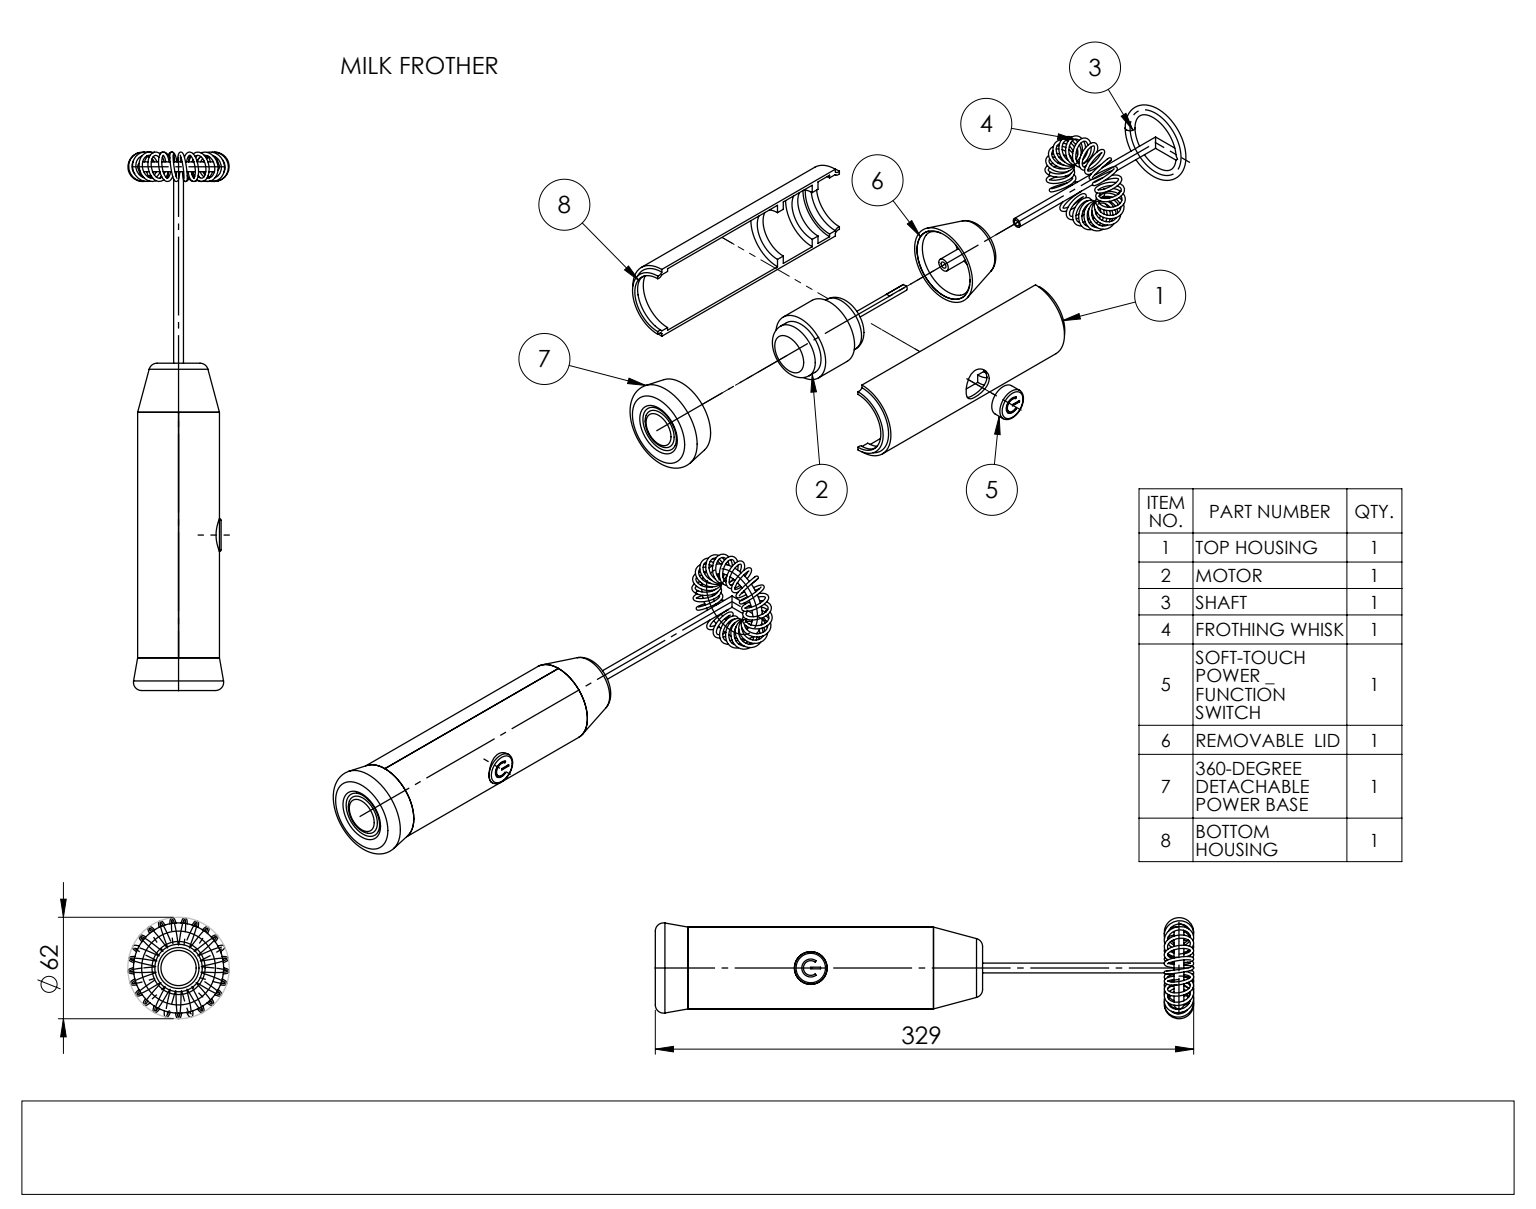
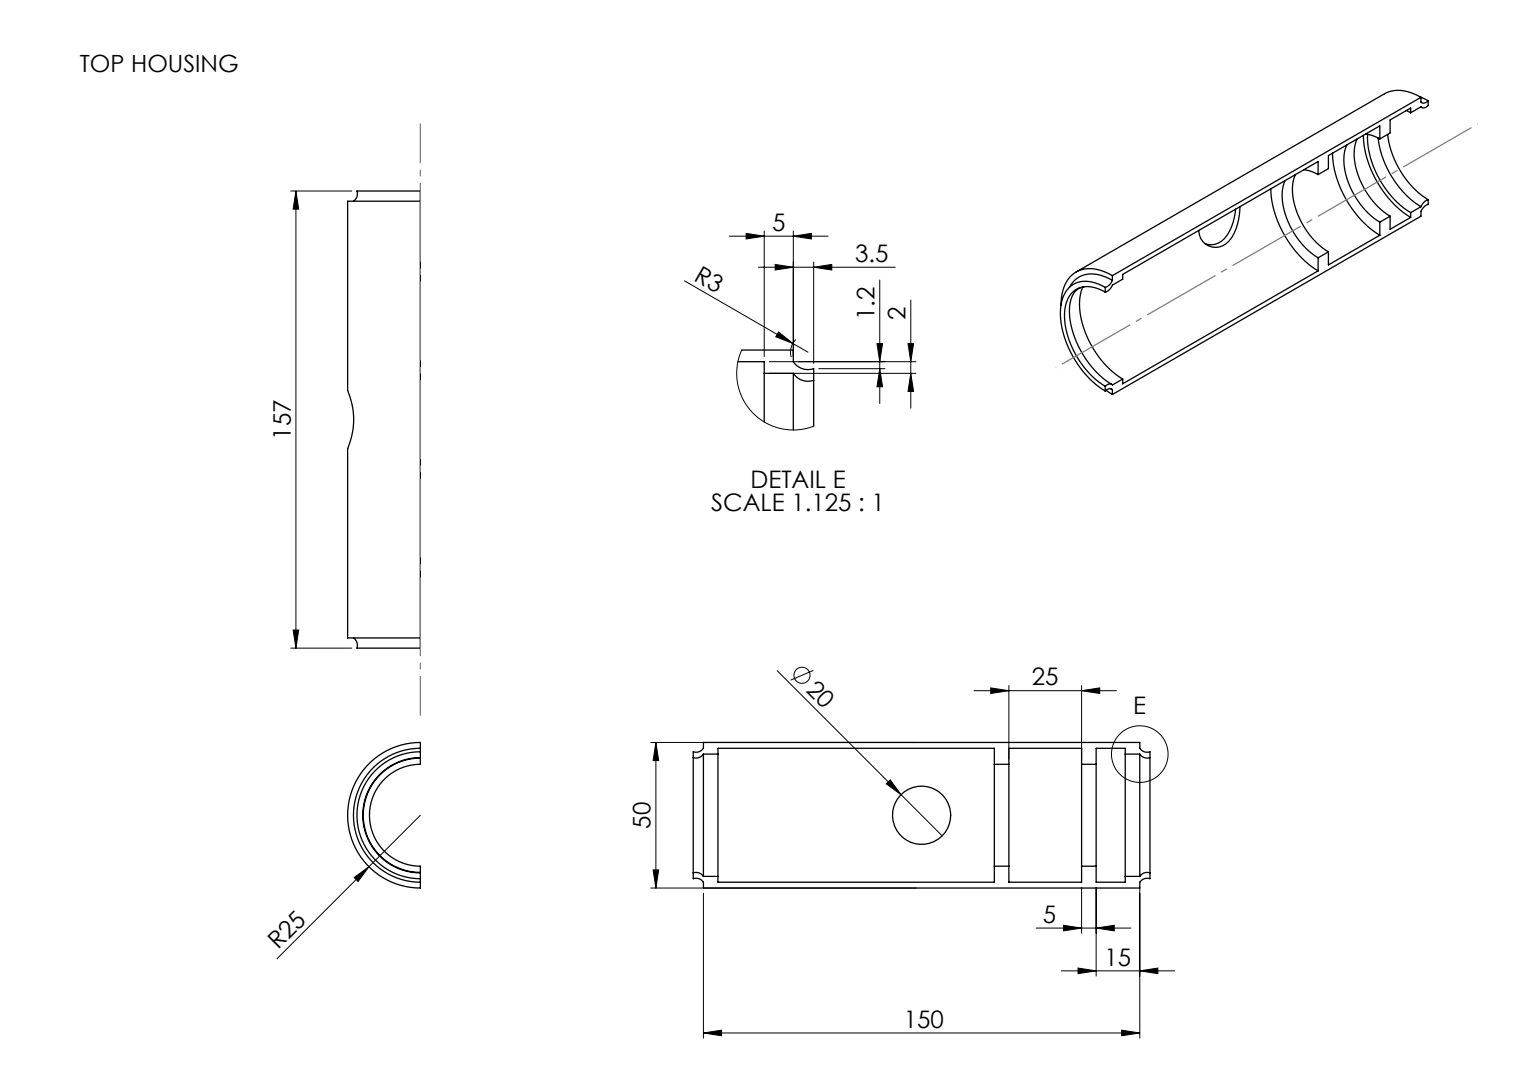
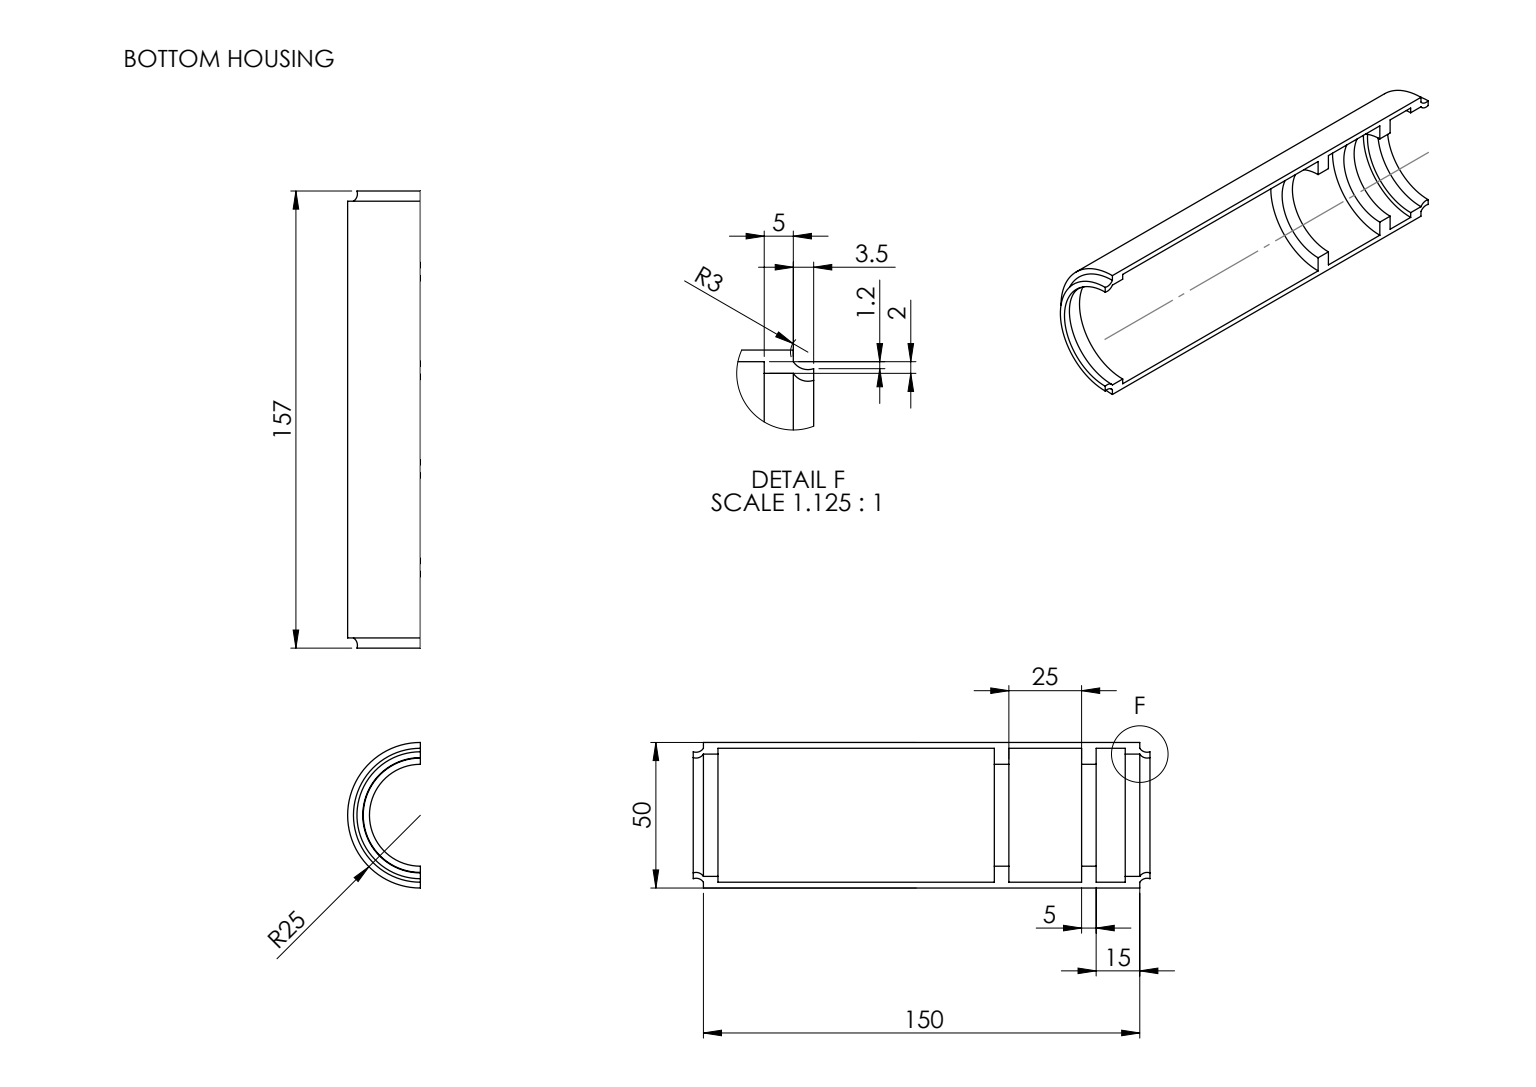
ISO-10303-21;
HEADER;
FILE_DESCRIPTION (('STEP AP214'),
    '1' );
FILE_NAME ('BR-822',
    '2026-10-08T15:02:10',
    ( '' ),
    ( '' ),
    'SwSTEP 2.0',
    'SolidWorks 2026',
    '' );
FILE_SCHEMA (( 'AUTOMOTIVE_DESIGN' ));
ENDSEC;

DATA;
#1 = CARTESIAN_POINT ( 'NONE',  ( -16.20471097821853235, -2.781505378741172319, -220.1484675126197317 ) ) ;
#2 = CARTESIAN_POINT ( 'NONE',  ( -19.86079186537285324, -0.7838168488858909821, -215.1601656726509475 ) ) ;
#3 = CARTESIAN_POINT ( 'NONE',  ( -18.57671526409105667, -15.84599122335686161, -218.9973662248357300 ) ) ;
#4 = SHAPE_REPRESENTATION_RELATIONSHIP ( 'NONE' , 'NONE' ,  #21505, #10999 ) ;
#5 = CARTESIAN_POINT ( 'NONE',  ( 13.07616324839670341, -23.69356132834180784, -230.7206382488779184 ) ) ;
#6 = CARTESIAN_POINT ( 'NONE',  ( -16.32047052250102581, 2.570795953410685009, -230.9329235942756213 ) ) ;
#7 = CARTESIAN_POINT ( 'NONE',  ( 10.40160332990717151, 27.59713857063802323, -221.5374724512453213 ) ) ;
#8 = CARTESIAN_POINT ( 'NONE',  ( -4.824452364631481416, 22.01523768541901305, -216.8350837474290245 ) ) ;
#9 = ORIENTED_EDGE ( 'NONE', *, *, #11620, .F. ) ;
#10 = CARTESIAN_POINT ( 'NONE',  ( 20.64894435305043174, -4.471500992710556233, -235.2405168901568686 ) ) ;
#11 = VERTEX_POINT ( 'NONE', #9296 ) ;
#12 = CARTESIAN_POINT ( 'NONE',  ( 12.99034161053428349, 11.71468708507361889, -230.9043293568357740 ) ) ;
#13 = CARTESIAN_POINT ( 'NONE',  ( -7.812160407601123069, 10.19183344000749081, -223.8148904943605828 ) ) ;
#14 = CARTESIAN_POINT ( 'NONE',  ( -12.30606003331388543, 10.59782772616791036, -231.0021630509705801 ) ) ;
#15 = CARTESIAN_POINT ( 'NONE',  ( -11.57846532275044460, -10.37575015818511304, -229.3776965522603462 ) ) ;
#16 = CARTESIAN_POINT ( 'NONE',  ( 2.465190328815661892E-29, 24.63401512838760610, -77.51594804401857175 ) ) ;
#17 = CARTESIAN_POINT ( 'NONE',  ( 16.21758812354607215, 4.665393561625732488, -232.5634757513959983 ) ) ;
#18 = CARTESIAN_POINT ( 'NONE',  ( -25.36936018126600345, 11.57160208538938306, -224.9662154788713622 ) ) ;
#19 = CARTESIAN_POINT ( 'NONE',  ( 16.71363093372661979, 20.70203100498337179, -215.6856694095356488 ) ) ;
#20 = CARTESIAN_POINT ( 'NONE',  ( 25.85597688020959239, 3.954559836939000039, -230.6766427064781624 ) ) ;
#21 = ADVANCED_FACE ( 'NONE', ( #14586 ), #5680, .F. ) ;
#22 = CARTESIAN_POINT ( 'NONE',  ( -4.451292041429703694, -15.86428280493796628, -231.0943874731633798 ) ) ;
#23 = ORIENTED_EDGE ( 'NONE', *, *, #2267, .F. ) ;
#24 = CARTESIAN_POINT ( 'NONE',  ( -8.978805095734141872, -14.89723076936793156, -219.0730636071341451 ) ) ;
#25 = CARTESIAN_POINT ( 'NONE',  ( -4.813101935419741295, 13.68373293383429434, -229.7840611589179503 ) ) ;
#26 = CARTESIAN_POINT ( 'NONE',  ( 1.541778504653760429, -23.48174737203985529, -233.9922866444541967 ) ) ;
#27 = CARTESIAN_POINT ( 'NONE',  ( -7.395406416482832590, 12.93623984139929739, -219.2606224730616873 ) ) ;
#28 = CARTESIAN_POINT ( 'NONE',  ( 22.70267758588118312, -6.899298642777032420, -215.6456595153534863 ) ) ;
#29 = AXIS2_PLACEMENT_3D ( 'NONE', #18064, #14475, #11199 ) ;
#30 = CARTESIAN_POINT ( 'NONE',  ( -13.52935284690462758, -5.503084506376929141, -222.3607690796775671 ) ) ;
#31 = CARTESIAN_POINT ( 'NONE',  ( -14.58575946311604277, 2.190332613129932327, -228.6717927865686590 ) ) ;
#32 = DIRECTION ( 'NONE',  ( -1.000000000000000000, 0.000000000000000000, 0.000000000000000000 ) ) ;
#33 = CARTESIAN_POINT ( 'NONE',  ( -3.139695637132168038, 25.12735071829084177, -230.1469660918596389 ) ) ;
#34 = CARTESIAN_POINT ( 'NONE',  ( 18.30177952310522471, 1.918278963380847468, -233.8574151782075887 ) ) ;
#35 = CARTESIAN_POINT ( 'NONE',  ( 7.639528166734322667, 11.92751229241157596, -224.6077814063189635 ) ) ;
#36 = CARTESIAN_POINT ( 'NONE',  ( 12.15450584778660570, 2.288537795953278220, -225.7049340319972828 ) ) ;
#37 = CARTESIAN_POINT ( 'NONE',  ( -3.630465294598614889, -13.73165509241056093, -221.1424077787270619 ) ) ;
#38 = CARTESIAN_POINT ( 'NONE',  ( 8.546572992885776543, 19.06776382077057974, -214.7173484156796519 ) ) ;
#39 = DIRECTION ( 'NONE',  ( -1.000000000000000000, 0.000000000000000000, 0.000000000000000000 ) ) ;
#40 = CARTESIAN_POINT ( 'NONE',  ( 8.654719819004025538, -19.13368099829532909, -232.5229659899653711 ) ) ;
#41 = CARTESIAN_POINT ( 'NONE',  ( -9.661739055621840322, 20.41227307912577871, -232.0920144483423257 ) ) ;
#42 = CARTESIAN_POINT ( 'NONE',  ( 3.192353461299334061, 22.13718518159985393, -217.1103300728619843 ) ) ;
#43 = CARTESIAN_POINT ( 'NONE',  ( -21.08965452150356867, -10.66825825602615296, -217.1903588586143314 ) ) ;
#44 = CARTESIAN_POINT ( 'NONE',  ( 28.65393683769942967, 4.398063292302325067, -219.1542358361629965 ) ) ;
#45 = CARTESIAN_POINT ( 'NONE',  ( 12.56362091610784049, 9.747446748398973071, -231.6428467497164547 ) ) ;
#46 = ORIENTED_EDGE ( 'NONE', *, *, #19993, .F. ) ;
#47 = CARTESIAN_POINT ( 'NONE',  ( 9.333020543840051531, 16.91085096921651143, -217.7308990335875762 ) ) ;
#48 = CARTESIAN_POINT ( 'NONE',  ( 25.31834813234691595, -9.473547856983202564, -230.2364162768838298 ) ) ;
#49 = CARTESIAN_POINT ( 'NONE',  ( 12.90474009670415967, -3.145873754258878385, -224.5449843457338375 ) ) ;
#50 = SURFACE_SIDE_STYLE ('',( #17385 ) ) ;
#51 = CARTESIAN_POINT ( 'NONE',  ( 13.61707622192329481, 14.84143455326118932, -217.6958999636067063 ) ) ;
#52 = CARTESIAN_POINT ( 'NONE',  ( -13.46535974834342220, -4.471564630954283359, -230.9063312536467834 ) ) ;
#53 = CARTESIAN_POINT ( 'NONE',  ( -6.870552667427666904, -18.85419487977974029, -216.2130481585807047 ) ) ;
#54 = CARTESIAN_POINT ( 'NONE',  ( 5.609436632608550966, -13.11664087352601094, -229.3324225951633650 ) ) ;
#55 = CARTESIAN_POINT ( 'NONE',  ( -1.364406401035816785, 24.33111505239456918, -219.5658712396381418 ) ) ;
#56 = CARTESIAN_POINT ( 'NONE',  ( 20.41968681625622040, 10.18377600976054076, -218.1989382652844256 ) ) ;
#57 = CARTESIAN_POINT ( 'NONE',  ( -26.58771759052039485, 5.114955214121561511, -218.2823714869195442 ) ) ;
#58 = CARTESIAN_POINT ( 'NONE',  ( -9.106229537879125147, 25.89784491087598184, -228.9807674929363372 ) ) ;
#59 = CARTESIAN_POINT ( 'NONE',  ( -21.75565187119130428, -2.221346625543990427, -217.0768970814220609 ) ) ;
#60 = ORIENTED_EDGE ( 'NONE', *, *, #7917, .F. ) ;
#61 = AXIS2_PLACEMENT_3D ( 'NONE', #8300, #8190, #21897 ) ;
#62 = CARTESIAN_POINT ( 'NONE',  ( -11.85645341316062051, 18.51497629668490674, -217.8828067666886454 ) ) ;
#63 = CARTESIAN_POINT ( 'NONE',  ( 15.88043104796248528, 11.88135572392608807, -216.2525917828042168 ) ) ;
#64 = CARTESIAN_POINT ( 'NONE',  ( 24.00840102751045890, 17.37402299239434100, -218.3110108534040137 ) ) ;
#65 = EDGE_CURVE ( 'NONE', #2304, #13811, #1543, .T. ) ;
#66 = CARTESIAN_POINT ( 'NONE',  ( 27.81506808824343580, -10.52944849582878106, -221.0913368219556503 ) ) ;
#67 = CARTESIAN_POINT ( 'NONE',  ( 1.322875655532295358, 1.500000000000000000, -105.0000000000000000 ) ) ;
#68 = VERTEX_POINT ( 'NONE', #19405 ) ;
#69 = CARTESIAN_POINT ( 'NONE',  ( -8.172572110426221670, 16.86653848210977813, -233.4220330256369493 ) ) ;
#70 = EDGE_CURVE ( 'NONE', #4018, #8552, #5732, .T. ) ;
#71 = CARTESIAN_POINT ( 'NONE',  ( -12.00435701841128022, -1.798699874815819166, -227.7674894005143074 ) ) ;
#72 = CARTESIAN_POINT ( 'NONE',  ( 0.000000000000000000, 24.63401512838747820, -77.51594804401857175 ) ) ;
#73 = VECTOR ( 'NONE', #4649, 1000.000000000000000 ) ;
#74 = CARTESIAN_POINT ( 'NONE',  ( 14.73698509926073186, 4.443590625350892331, -227.4062002049096236 ) ) ;
#75 = CARTESIAN_POINT ( 'NONE',  ( -13.69675006931110417, 3.702342960760605539, -228.0723273272095355 ) ) ;
#76 = CARTESIAN_POINT ( 'NONE',  ( 9.104026917753444081, -10.66572815660443041, -221.9193219976906448 ) ) ;
#77 = DIRECTION ( 'NONE',  ( 1.000000000000000000, 0.000000000000000000, 0.000000000000000000 ) ) ;
#78 = CARTESIAN_POINT ( 'NONE',  ( -27.82842955277035202, 11.70195273568964112, -227.9294339757464911 ) ) ;
#79 = PRODUCT_DEFINITION_SHAPE ( 'NONE', 'NONE',  #8374 ) ;
#80 = CARTESIAN_POINT ( 'NONE',  ( -15.15434969228324924, 4.423874646950748613, -230.6144467931089821 ) ) ;
#81 = CARTESIAN_POINT ( 'NONE',  ( 1.102456202203287550, -23.13885590315818064, -232.0370787247644557 ) ) ;
#82 = CIRCLE ( 'NONE', #20492, 19.79999999999999716 ) ;
#83 = CARTESIAN_POINT ( 'NONE',  ( 12.50000000000000355, 0.000000000000000000, -65.00000000000000000 ) ) ;
#84 = DIRECTION ( 'NONE',  ( 0.000000000000000000, 1.000000000000000000, 0.000000000000000000 ) ) ;
#85 = CARTESIAN_POINT ( 'NONE',  ( -28.13472254077564116, 12.33996625515159629, -224.9141344439281909 ) ) ;
#86 = CARTESIAN_POINT ( 'NONE',  ( 17.16551562789753049, -17.52877442517796780, -218.8649675774640286 ) ) ;
#87 = CARTESIAN_POINT ( 'NONE',  ( 12.82607305708569889, -2.701876713238477556, -226.3171933651010761 ) ) ;
#88 = AXIS2_PLACEMENT_3D ( 'NONE', #22054, #11930, #10248 ) ;
#89 = CARTESIAN_POINT ( 'NONE',  ( 18.76166303929371537, -3.000000000000002665, -225.0000000000001990 ) ) ;
#90 = CARTESIAN_POINT ( 'NONE',  ( 10.01015180241662605, 20.19019600914695900, -219.1042218506083543 ) ) ;
#91 = AXIS2_PLACEMENT_3D ( 'NONE', #18121, #12939, #8104 ) ;
#92 = CARTESIAN_POINT ( 'NONE',  ( 14.78510113471881304, 14.77128235908076803, -230.8056908117964383 ) ) ;
#93 = CARTESIAN_POINT ( 'NONE',  ( -2.652888268066178945, -28.18865072326549637, -221.4226523288203623 ) ) ;
#94 = CARTESIAN_POINT ( 'NONE',  ( 15.54083024098960486, -10.44392130763852222, -217.6620978190037476 ) ) ;
#95 = ORIENTED_EDGE ( 'NONE', *, *, #2038, .F. ) ;
#96 = CARTESIAN_POINT ( 'NONE',  ( -12.43544732248594720, 12.69828336922617318, -219.3367909706387877 ) ) ;
#97 = CARTESIAN_POINT ( 'NONE',  ( -24.92290506463145405, 6.124412323591598373, -220.3779252408000104 ) ) ;
#98 = CARTESIAN_POINT ( 'NONE',  ( -12.45629340980802269, 5.675423426979704367, -220.8874502847910719 ) ) ;
#99 = ORIENTED_EDGE ( 'NONE', *, *, #17132, .T. ) ;
#100 = CARTESIAN_POINT ( 'NONE',  ( -11.04629350503636864, -16.47921676447750983, -219.6257371594006145 ) ) ;
#101 = CARTESIAN_POINT ( 'NONE',  ( -0.6349943332661909245, -10.75744069813302417, 92.00000000000001421 ) ) ;
#102 = ORIENTED_EDGE ( 'NONE', *, *, #14912, .T. ) ;
#103 = CARTESIAN_POINT ( 'NONE',  ( 22.37138132874926910, 6.723028048925958622, -217.7073806909121743 ) ) ;
#104 = CARTESIAN_POINT ( 'NONE',  ( 19.38320831645075870, -15.01455373846949293, -219.3474289024948689 ) ) ;
#105 = CARTESIAN_POINT ( 'NONE',  ( 4.603870848087811218, 30.13529352683433515, -225.9623629403671430 ) ) ;
#106 = CARTESIAN_POINT ( 'NONE',  ( -16.65698539163286540, 11.03290537638306112, -233.6474915129378758 ) ) ;
#107 = VECTOR ( 'NONE', #10777, 1000.000000000000000 ) ;
#108 = AXIS2_PLACEMENT_3D ( 'NONE', #21877, #21538, #9854 ) ;
#109 = CARTESIAN_POINT ( 'NONE',  ( 12.66989206167516357, 2.082990619159506007, -225.6419847029432901 ) ) ;
#110 = PRODUCT_DEFINITION ( 'UNKNOWN', '', #959, #2880 ) ;
#111 = CARTESIAN_POINT ( 'NONE',  ( 7.168644370073567806, 19.32044210858112265, -233.1278450877711634 ) ) ;
#112 = CARTESIAN_POINT ( 'NONE',  ( 22.03647168420945590, 0.3315607655625663064, -232.0572713672586644 ) ) ;
#113 = CARTESIAN_POINT ( 'NONE',  ( 6.589392574981438599, -17.08498810221841069, -232.9613445306918322 ) ) ;
#114 = CARTESIAN_POINT ( 'NONE',  ( 14.31589812732703670, -5.349901619299376243, -221.2752230612865105 ) ) ;
#115 = CARTESIAN_POINT ( 'NONE',  ( 23.92685091328690916, 0.000000000000000000, 80.43141006107198621 ) ) ;
#116 = DIRECTION ( 'NONE',  ( -1.000000000000000000, 0.000000000000000000, 0.000000000000000000 ) ) ;
#117 = CARTESIAN_POINT ( 'NONE',  ( 15.01439307471096463, 1.118969480519667048, -226.7488225241675366 ) ) ;
#118 = CARTESIAN_POINT ( 'NONE',  ( -15.02551512915570697, -20.93241195546420741, -218.9083119944682778 ) ) ;
#119 = VECTOR ( 'NONE', #1597, 1000.000000000000000 ) ;
#120 = CIRCLE ( 'NONE', #7315, 21.50000000000000711 ) ;
#121 = CARTESIAN_POINT ( 'NONE',  ( -22.13857085231108712, 6.545953331035805789, -217.2801712530867633 ) ) ;
#122 = CARTESIAN_POINT ( 'NONE',  ( -0.3197916200495275474, 16.38897215927557482, -229.9606066735827028 ) ) ;
#123 = CARTESIAN_POINT ( 'NONE',  ( 2.085064686336211892, 14.99578618537741548, -226.0985834012817861 ) ) ;
#124 = CARTESIAN_POINT ( 'NONE',  ( -27.59531865868800082, -2.367229732415436771, -222.8128998708299093 ) ) ;
#125 = CARTESIAN_POINT ( 'NONE',  ( 7.995304978256253747, 13.28024228361502779, -220.6535174700288451 ) ) ;
#126 = CARTESIAN_POINT ( 'NONE',  ( -10.95054816480499760, 8.339404316518379545, -224.1596700080921778 ) ) ;
#127 = CARTESIAN_POINT ( 'NONE',  ( -16.40443871513620522, 4.023423476741658789, -228.9829044427089002 ) ) ;
#128 = CARTESIAN_POINT ( 'NONE',  ( -11.18311023676720062, -15.30649302686804347, -231.8766562234714002 ) ) ;
#129 = CARTESIAN_POINT ( 'NONE',  ( 26.00000000000000000, -0.5000000000000000000, 0.000000000000000000 ) ) ;
#130 = CARTESIAN_POINT ( 'NONE',  ( 20.76808360334631232, 5.412616674732960931, -234.1222385626545304 ) ) ;
#131 = AXIS2_PLACEMENT_3D ( 'NONE', #8453, #22168, #4530 ) ;
#132 = CARTESIAN_POINT ( 'NONE',  ( -14.22959263369750182, 18.28478771081826793, -217.8090497856120464 ) ) ;
#133 = CIRCLE ( 'NONE', #6226, 27.49181041625929112 ) ;
#134 = CARTESIAN_POINT ( 'NONE',  ( 5.964915545484365644, 11.50358694729900577, -229.9646467236423462 ) ) ;
#135 = CARTESIAN_POINT ( 'NONE',  ( -21.08008464085897060, -0.9048411197481797119, -217.0000000010748522 ) ) ;
#136 = CARTESIAN_POINT ( 'NONE',  ( -20.47121909278842722, -2.147015668718357695, -235.2226201655121258 ) ) ;
#137 = VERTEX_POINT ( 'NONE', #405 ) ;
#138 = CARTESIAN_POINT ( 'NONE',  ( -28.43596199216294806, -10.51226423640377838, -227.0041752157952430 ) ) ;
#139 = CARTESIAN_POINT ( 'NONE',  ( -15.64710113362562183, 25.90300453978063189, -220.8637308366217269 ) ) ;
#140 = CARTESIAN_POINT ( 'NONE',  ( -5.525229149912007642, -13.32411127922494742, -220.4018445532201440 ) ) ;
#141 = CARTESIAN_POINT ( 'NONE',  ( -4.620781219515533778, 16.99182040716223696, -217.1278208835672672 ) ) ;
#142 = CARTESIAN_POINT ( 'NONE',  ( 29.03861746756086859, -6.579333063807603743, -229.8282242506458317 ) ) ;
#143 = CARTESIAN_POINT ( 'NONE',  ( -29.22168435891936156, -1.352755938724206519, -225.9547066689444250 ) ) ;
#144 = CARTESIAN_POINT ( 'NONE',  ( 29.81944548462877975, 8.043843257819576209, -228.1755181449411793 ) ) ;
#145 = FACE_OUTER_BOUND ( 'NONE', #18733, .T. ) ;
#146 = CARTESIAN_POINT ( 'NONE',  ( -0.7879796667336372851, 21.22375955577181372, -219.1554080315090118 ) ) ;
#147 = CARTESIAN_POINT ( 'NONE',  ( -29.16153046926437753, 6.356672163541281506, -226.4393515956758165 ) ) ;
#148 = CARTESIAN_POINT ( 'NONE',  ( 18.76922974182421555, 13.12635134380198210, -217.8010375391909008 ) ) ;
#149 = CARTESIAN_POINT ( 'NONE',  ( 19.55931020704464274, 3.833820734573247346, -215.4549349108404783 ) ) ;
#150 = CARTESIAN_POINT ( 'NONE',  ( 3.585135836405817233, -11.76492230538331896, -228.1718440842192024 ) ) ;
#151 = CARTESIAN_POINT ( 'NONE',  ( 1.660345614755502686, 12.19060476922103931, -223.1112690039082906 ) ) ;
#152 = AXIS2_PLACEMENT_3D ( 'NONE', #2857, #13336, #13120 ) ;
#153 = CARTESIAN_POINT ( 'NONE',  ( 1.387778780781446180E-13, -19.80000000000006111, 78.50000000000000000 ) ) ;
#154 = CARTESIAN_POINT ( 'NONE',  ( 0.5037192024386412115, -21.28831724695581684, -215.7417742237681466 ) ) ;
#155 = CARTESIAN_POINT ( 'NONE',  ( -8.317278876689359279, 23.15034512777772235, -218.2935523245793092 ) ) ;
#156 = CARTESIAN_POINT ( 'NONE',  ( 14.20064147608437821, 14.63411858269657806, -233.6150408276221242 ) ) ;
#157 = CARTESIAN_POINT ( 'NONE',  ( -26.43144772945995413, -6.745116643720071359, -219.5134289301136050 ) ) ;
#158 = CARTESIAN_POINT ( 'NONE',  ( -22.38528940623734798, 16.50235888036280230, -227.1443357386333162 ) ) ;
#159 = CARTESIAN_POINT ( 'NONE',  ( -17.89085717681497201, 10.08962028281416856, -232.3705156551908431 ) ) ;
#160 = CARTESIAN_POINT ( 'NONE',  ( 27.79670308438203108, 10.67628923451848877, -225.2981230784098727 ) ) ;
#161 = VERTEX_POINT ( 'NONE', #16052 ) ;
#162 = CARTESIAN_POINT ( 'NONE',  ( 12.23063869552301242, 12.84118223717021934, -218.8273164334868284 ) ) ;
#163 = CARTESIAN_POINT ( 'NONE',  ( 10.59565547865383728, -13.75865772189005476, -221.5384683668846435 ) ) ;
#164 = ORIENTED_EDGE ( 'NONE', *, *, #3485, .T. ) ;
#165 = CARTESIAN_POINT ( 'NONE',  ( 27.76845665997775114, -9.103683020204879739, -229.9743915588940979 ) ) ;
#166 = CARTESIAN_POINT ( 'NONE',  ( -0.6272116608575281083, 20.18031380156121202, -219.3960054794027030 ) ) ;
#167 = ORIENTED_EDGE ( 'NONE', *, *, #18433, .F. ) ;
#168 = SURFACE_STYLE_USAGE ( .BOTH. , #50 ) ;
#169 = AXIS2_PLACEMENT_3D ( 'NONE', #2504, #9798, #9382 ) ;
#170 = CARTESIAN_POINT ( 'NONE',  ( 23.04897566969193079, 17.95862962700741861, -223.6438515760422661 ) ) ;
#171 = CARTESIAN_POINT ( 'NONE',  ( -11.65988442122670676, -3.998659314375652141, -223.4258670541443621 ) ) ;
#172 = CARTESIAN_POINT ( 'NONE',  ( -5.902479482706956659, -14.78727544128710214, -218.5565286504736946 ) ) ;
#173 = CARTESIAN_POINT ( 'NONE',  ( 13.04434844185555420, -10.19049307777131297, -230.8679447648462713 ) ) ;
#174 = CARTESIAN_POINT ( 'NONE',  ( -7.366083718505351818, 19.86648438590005838, -231.8662444779758971 ) ) ;
#175 = CARTESIAN_POINT ( 'NONE',  ( 26.00000000000000000, 0.5000000000000000000, 0.000000000000000000 ) ) ;
#176 = CARTESIAN_POINT ( 'NONE',  ( 17.02590609996173754, 6.796709046606974169, -230.8496778635019098 ) ) ;
#177 = CARTESIAN_POINT ( 'NONE',  ( -13.55591840520136770, 8.363404288414606924, -231.2690188357804857 ) ) ;
#178 = CARTESIAN_POINT ( 'NONE',  ( -5.589224416770360193, 14.13652937339764115, -225.1481999119820330 ) ) ;
#179 = ORIENTED_EDGE ( 'NONE', *, *, #598, .F. ) ;
#180 = CARTESIAN_POINT ( 'NONE',  ( 5.359747511823000465, 20.14556701535824601, -232.9094821222151381 ) ) ;
#181 = CARTESIAN_POINT ( 'NONE',  ( -18.90911063232017142, 5.352531560950812839, -219.6301177803536575 ) ) ;
#182 = CARTESIAN_POINT ( 'NONE',  ( 13.85207896949186335, 7.847214149978243292, -217.3457543576531066 ) ) ;
#183 = CARTESIAN_POINT ( 'NONE',  ( 5.133806223762193532, -16.42362916962670383, -230.4968203642818310 ) ) ;
#184 = DIRECTION ( 'NONE',  ( 0.000000000000000000, 0.000000000000000000, -1.000000000000000000 ) ) ;
#185 = ORIENTED_EDGE ( 'NONE', *, *, #19709, .T. ) ;
#186 = ADVANCED_FACE ( 'NONE', ( #19627 ), #432, .T. ) ;
#187 = CARTESIAN_POINT ( 'NONE',  ( -6.101488798441174310, 11.33371047077072369, -225.3616985956418546 ) ) ;
#188 = CARTESIAN_POINT ( 'NONE',  ( -25.17982544627478703, 0.9072515815786372784, -215.5253307415545692 ) ) ;
#189 = CARTESIAN_POINT ( 'NONE',  ( 26.48152825632016061, -2.044474411990439666, -219.3412966555575565 ) ) ;
#190 = CARTESIAN_POINT ( 'NONE',  ( 25.69300549816939494, 5.947472783069708946, -230.6131061331718115 ) ) ;
#191 = FACE_OUTER_BOUND ( 'NONE', #11098, .T. ) ;
#192 = CIRCLE ( 'NONE', #12763, 23.92685091328691271 ) ;
#193 = CARTESIAN_POINT ( 'NONE',  ( 20.25084204406298127, -10.11176871144018818, -232.7817218064674591 ) ) ;
#194 = CARTESIAN_POINT ( 'NONE',  ( -8.823862513872974489, 14.92351368520778898, -217.1499513473673346 ) ) ;
#195 = CARTESIAN_POINT ( 'NONE',  ( -28.17543631911187063, 3.557555778861649642, -230.1980773687482156 ) ) ;
#196 = CARTESIAN_POINT ( 'NONE',  ( -1.432270239486107766, -17.91381153981195951, -219.1344183636291802 ) ) ;
#197 = CARTESIAN_POINT ( 'NONE',  ( 0.000000000000000000, 0.000000000000000000, 78.50000000000000000 ) ) ;
#198 = EDGE_CURVE ( 'NONE', #16686, #4564, #9428, .T. ) ;
#199 = LINE ( 'NONE', #7182, #5891 ) ;
#200 = CARTESIAN_POINT ( 'NONE',  ( -20.18153419852512442, 14.25141268122526483, -233.5059133483111964 ) ) ;
#201 = CARTESIAN_POINT ( 'NONE',  ( 23.31955656579280145, -13.39010844438576520, -228.3495985225334266 ) ) ;
#202 = CARTESIAN_POINT ( 'NONE',  ( -27.85133024402786006, -1.794102530182491773, -229.4204807338591081 ) ) ;
#203 = CARTESIAN_POINT ( 'NONE',  ( -22.92002576459826102, 9.983672621040497575, 0.6612741795047580862 ) ) ;
#204 = CARTESIAN_POINT ( 'NONE',  ( 24.14003655968566520, 13.76285650325712773, -228.1266575292093819 ) ) ;
#205 = CARTESIAN_POINT ( 'NONE',  ( -4.813101935419741295, 13.68373293383429434, -229.7840611589179503 ) ) ;
#206 = CARTESIAN_POINT ( 'NONE',  ( 17.42772712443221650, 11.35756022693713341, -231.2166398222404382 ) ) ;
#207 = CARTESIAN_POINT ( 'NONE',  ( -7.194605141218047173, -25.04260655977047278, -230.2952862975163271 ) ) ;
#208 = CIRCLE ( 'NONE', #12782, 23.00000000000000000 ) ;
#209 = CARTESIAN_POINT ( 'NONE',  ( 23.45680152528306550, 2.072154465955917235, -232.7243927205664704 ) ) ;
#210 = ORIENTED_EDGE ( 'NONE', *, *, #8940, .F. ) ;
#211 = CIRCLE ( 'NONE', #21742, 17.50000000000000711 ) ;
#212 = CARTESIAN_POINT ( 'NONE',  ( 2.579827969572558111, 15.91317371615649101, -219.7652087782269916 ) ) ;
#213 = CARTESIAN_POINT ( 'NONE',  ( -22.90687623753526125, 9.466200233939549236, -230.1557007022273638 ) ) ;
#214 = CARTESIAN_POINT ( 'NONE',  ( -30.35034897870229287, 7.696526532841741819, -221.5749790623549416 ) ) ;
#215 = VERTEX_POINT ( 'NONE', #16158 ) ;
#216 = CARTESIAN_POINT ( 'NONE',  ( -12.46707500365009480, -15.03319212650626824, -230.3369784839848933 ) ) ;
#217 = CARTESIAN_POINT ( 'NONE',  ( 0.000000000000000000, 0.000000000000000000, 75.00000000000000000 ) ) ;
#218 = ORIENTED_EDGE ( 'NONE', *, *, #19552, .T. ) ;
#219 = CARTESIAN_POINT ( 'NONE',  ( 24.78222556642275620, 17.97262539535998371, -226.6641400693514470 ) ) ;
#220 = CARTESIAN_POINT ( 'NONE',  ( 18.79065350309113214, -20.33706828427738600, -226.6662063318914591 ) ) ;
#221 = CARTESIAN_POINT ( 'NONE',  ( 23.49048926389013658, 9.645778135078892035, -218.7307869890797463 ) ) ;
#222 = CARTESIAN_POINT ( 'NONE',  ( -16.39453490553961856, 20.24836633112041184, -233.1722131570092245 ) ) ;
#223 = VECTOR ( 'NONE', #786, 1000.000000000000000 ) ;
#224 = CARTESIAN_POINT ( 'NONE',  ( 14.54999166170408209, 3.068772298969228096, -219.4784171371563275 ) ) ;
#225 = AXIS2_PLACEMENT_3D ( 'NONE', #7569, #15900, #3952 ) ;
#226 = CARTESIAN_POINT ( 'NONE',  ( 13.43170911749896490, 19.07691563292472026, -232.7497845103644636 ) ) ;
#227 = DIRECTION ( 'NONE',  ( -1.000000000000000000, 0.000000000000000000, -0.000000000000000000 ) ) ;
#228 = CARTESIAN_POINT ( 'NONE',  ( 6.427665535191954937, -16.40046818492683656, -232.5919299485929912 ) ) ;
#229 = CARTESIAN_POINT ( 'NONE',  ( 11.43609017326686050, -13.06727081285745307, -217.8903327850316316 ) ) ;
#230 = DIRECTION ( 'NONE',  ( 0.000000000000000000, -1.000000000000000000, 0.000000000000000000 ) ) ;
#231 = DIRECTION ( 'NONE',  ( -2.162300680179923768E-16, -1.000000000000000000, 0.000000000000000000 ) ) ;
#232 = CARTESIAN_POINT ( 'NONE',  ( -23.95129667199961077, 20.99391807043993552, -227.1541646794576081 ) ) ;
#233 = CARTESIAN_POINT ( 'NONE',  ( -22.78589867900506150, -1.373495078166624861, -218.8339345403132370 ) ) ;
#234 = CARTESIAN_POINT ( 'NONE',  ( 30.47710800431509170, 7.409378661937554789, -223.2007768404241688 ) ) ;
#235 = CARTESIAN_POINT ( 'NONE',  ( -1.301562195391901877, 16.19210386685474390, -220.0867867038183192 ) ) ;
#236 = CARTESIAN_POINT ( 'NONE',  ( 1.847452069095833593, 15.11597492720254543, -223.6261404253179421 ) ) ;
#237 = VERTEX_POINT ( 'NONE', #7603 ) ;
#238 = CARTESIAN_POINT ( 'NONE',  ( 14.54962894845190036, -2.357901078066860112, -232.0046840244626765 ) ) ;
#239 = CIRCLE ( 'NONE', #21420, 3.000000000000002665 ) ;
#240 = CARTESIAN_POINT ( 'NONE',  ( 22.66390650824515873, 11.48342577402021725, -231.3155567808436217 ) ) ;
#241 = CARTESIAN_POINT ( 'NONE',  ( -11.10182655035041144, 8.778638955377752850, -227.1050196202568827 ) ) ;
#242 = CARTESIAN_POINT ( 'NONE',  ( -12.26337789213896201, 9.274758280606999250, -219.9806108963443876 ) ) ;
#243 = CARTESIAN_POINT ( 'NONE',  ( -24.60063047153272819, -17.11178239752603858, -226.7032704813509554 ) ) ;
#244 = CARTESIAN_POINT ( 'NONE',  ( -16.63766460830045091, 5.158675778507696208, -232.1659425527909093 ) ) ;
#245 = CARTESIAN_POINT ( 'NONE',  ( -23.00000000000000000, 0.000000000000000000, 75.00000000000000000 ) ) ;
#246 = FACE_OUTER_BOUND ( 'NONE', #1813, .T. ) ;
#247 = CARTESIAN_POINT ( 'NONE',  ( 0.000000000000000000, 0.000000000000000000, -120.0000000000000142 ) ) ;
#248 = CARTESIAN_POINT ( 'NONE',  ( -12.04619960554013502, 10.22290173510000777, -223.1766370265664534 ) ) ;
#249 = CARTESIAN_POINT ( 'NONE',  ( 25.41781277602550304, 19.49958712797920057, -223.1230538376805441 ) ) ;
#250 = EDGE_CURVE ( 'NONE', #10146, #1916, #14804, .T. ) ;
#251 = CARTESIAN_POINT ( 'NONE',  ( 27.84414217501293010, 2.965433895642837214, -221.8999927093654492 ) ) ;
#252 = CARTESIAN_POINT ( 'NONE',  ( -13.00317340065129557, -2.278067296278880161, -219.8118061108488916 ) ) ;
#253 = EDGE_LOOP ( 'NONE', ( #21985, #19311, #21733, #15919, #6601, #3460 ) ) ;
#254 = CARTESIAN_POINT ( 'NONE',  ( -23.08212926897555306, -14.71479305961103101, -218.7697472404056214 ) ) ;
#255 = CARTESIAN_POINT ( 'NONE',  ( -7.312583518931054627, 16.22063427959223958, -217.3454962955413521 ) ) ;
#256 = CARTESIAN_POINT ( 'NONE',  ( -14.34280792637948743, -22.10828917559366147, -217.4172704053049756 ) ) ;
#257 = CARTESIAN_POINT ( 'NONE',  ( 7.743212835174657194, 11.90778931056080481, -226.0491028376908105 ) ) ;
#258 = CARTESIAN_POINT ( 'NONE',  ( 6.415926650623908323, -16.27382107952271895, -215.7995092914603674 ) ) ;
#259 = CARTESIAN_POINT ( 'NONE',  ( 14.03461600111380037, -0.1787097712218918000, -227.9951367205099473 ) ) ;
#260 = CARTESIAN_POINT ( 'NONE',  ( -28.61025869263052712, 6.891613135096296361, -222.2489362813765013 ) ) ;
#261 = CARTESIAN_POINT ( 'NONE',  ( -5.764806379010653181, 14.19340719117484007, -223.8851086052821415 ) ) ;
#262 = CARTESIAN_POINT ( 'NONE',  ( 26.06405806384012536, 5.488112530166501024, -216.5020692413490622 ) ) ;
#263 = CARTESIAN_POINT ( 'NONE',  ( -13.56011990957801139, -0.3895158544032599202, -219.3211261236655218 ) ) ;
#264 = CARTESIAN_POINT ( 'NONE',  ( 12.79953165872901266, 10.20044330008568778, -230.3912386799665626 ) ) ;
#265 = CARTESIAN_POINT ( 'NONE',  ( -0.4062606655315902371, -23.43967590431752512, -234.4451928229410100 ) ) ;
#266 = CARTESIAN_POINT ( 'NONE',  ( 5.264801124131998300, 10.54092478143144795, -226.4890466082630098 ) ) ;
#267 = CARTESIAN_POINT ( 'NONE',  ( 21.31262902390056624, 0.4111834581965390645, -232.0572713672585792 ) ) ;
#268 = CARTESIAN_POINT ( 'NONE',  ( 0.2152704783746036410, -12.84635275796930642, -226.1081088095504015 ) ) ;
#269 = CARTESIAN_POINT ( 'NONE',  ( -11.85645341316062051, 18.51497629668490674, -217.8828067666886454 ) ) ;
#270 = CARTESIAN_POINT ( 'NONE',  ( 12.74913679152205148, 9.185760885856177893, -218.6542381594888980 ) ) ;
#271 = CARTESIAN_POINT ( 'NONE',  ( -27.88251101234890328, -7.575382714962081820, -221.6715981084135478 ) ) ;
#272 = CARTESIAN_POINT ( 'NONE',  ( -18.90911063232017142, 5.352531560950812839, -219.6301177803536575 ) ) ;
#273 = EDGE_CURVE ( 'NONE', #12453, #12432, #18177, .T. ) ;
#274 = CARTESIAN_POINT ( 'NONE',  ( -4.678665819194652187, 12.50541869316310262, -220.1509054161798247 ) ) ;
#275 = CARTESIAN_POINT ( 'NONE',  ( 13.89183999136464820, 6.553741795688899252, -220.8646181278399752 ) ) ;
#276 = ORIENTED_EDGE ( 'NONE', *, *, #16709, .F. ) ;
#277 = CARTESIAN_POINT ( 'NONE',  ( 10.85678324124089755, -13.97331853324622131, -221.1336851750754420 ) ) ;
#278 = ORIENTED_EDGE ( 'NONE', *, *, #1896, .T. ) ;
#279 = CARTESIAN_POINT ( 'NONE',  ( 5.511302051500400090, -18.01881380728196902, -231.5522404100356084 ) ) ;
#280 = CARTESIAN_POINT ( 'NONE',  ( -7.928079932584687128, 26.12067226064367986, -221.2051195461628197 ) ) ;
#281 = ORIENTED_EDGE ( 'NONE', *, *, #14770, .F. ) ;
#282 = SURFACE_STYLE_FILL_AREA ( #6812 ) ;
#283 = CARTESIAN_POINT ( 'NONE',  ( 21.25094435758043332, 17.68230636442804027, -229.7964888993842010 ) ) ;
#284 = CARTESIAN_POINT ( 'NONE',  ( 26.54225689383817866, -6.924125931238839016, -230.1506921200174247 ) ) ;
#285 = CARTESIAN_POINT ( 'NONE',  ( -1.632242579688942596, -13.62074943359385415, -221.1585305289511041 ) ) ;
#286 = CARTESIAN_POINT ( 'NONE',  ( -3.300598509645395584, -18.18730530649546395, -233.4303386612170925 ) ) ;
#287 = CARTESIAN_POINT ( 'NONE',  ( -2.015708574708954259, 26.78900769828807782, -221.5371848586876808 ) ) ;
#288 = DIRECTION ( 'NONE',  ( -1.000000000000000000, 0.000000000000000000, 0.000000000000000000 ) ) ;
#289 = CARTESIAN_POINT ( 'NONE',  ( 17.24423567610276109, 8.542587572837451404, -218.6562240232607621 ) ) ;
#290 = CARTESIAN_POINT ( 'NONE',  ( -11.26857159993117996, 28.96895336474501192, -225.6039696848669678 ) ) ;
#291 = CARTESIAN_POINT ( 'NONE',  ( -8.463283775975803280, 12.69606588598396613, -228.6351674091961286 ) ) ;
#292 = ORIENTED_EDGE ( 'NONE', *, *, #18240, .F. ) ;
#293 = CARTESIAN_POINT ( 'NONE',  ( -1.433739110790628102, 17.19322394474796667, -219.1420620387681879 ) ) ;
#294 = CARTESIAN_POINT ( 'NONE',  ( -16.37512411505367282, 2.406627362596846620, -227.7341547288202719 ) ) ;
#295 = CARTESIAN_POINT ( 'NONE',  ( 7.651502705057454889, 16.60422307457919544, -215.4679461133464144 ) ) ;
#296 = CARTESIAN_POINT ( 'NONE',  ( 5.452943511046377090, -14.64908918772281865, -221.6090591728701611 ) ) ;
#297 = DIRECTION ( 'NONE',  ( 0.000000000000000000, 0.000000000000000000, 1.000000000000000000 ) ) ;
#298 = ORIENTED_EDGE ( 'NONE', *, *, #2080, .T. ) ;
#299 = CARTESIAN_POINT ( 'NONE',  ( -11.69688825528096388, 18.63404371591177622, -215.8612738028812714 ) ) ;
#300 = CARTESIAN_POINT ( 'NONE',  ( 21.83031488338151149, -1.542591969257156803, -231.3901500139511427 ) ) ;
#301 = CARTESIAN_POINT ( 'NONE',  ( 27.02029988085337919, -0.4174685747284823112, -230.1188858631967378 ) ) ;
#302 = CARTESIAN_POINT ( 'NONE',  ( 13.03557269046774714, 7.519834803053426775, -226.9490612297269081 ) ) ;
#303 = CARTESIAN_POINT ( 'NONE',  ( -13.65925618638770800, 3.289586759644148817, -222.1579143493116533 ) ) ;
#304 = CARTESIAN_POINT ( 'NONE',  ( 5.451525948382545117, -12.45300865616632713, -227.8545162512558306 ) ) ;
#305 = CARTESIAN_POINT ( 'NONE',  ( 0.000000000000000000, 0.000000000000000000, 0.000000000000000000 ) ) ;
#306 = CARTESIAN_POINT ( 'NONE',  ( -10.30050448363967419, 10.07750059423401190, -220.1837019037183723 ) ) ;
#307 = CARTESIAN_POINT ( 'NONE',  ( -12.80532875684362715, 24.61139456694233374, -232.5885756414849084 ) ) ;
#308 = CARTESIAN_POINT ( 'NONE',  ( -16.71711190488355570, 0.6105529133557690002, -230.9511258789794681 ) ) ;
#309 = CARTESIAN_POINT ( 'NONE',  ( -13.02663300398358892, -17.15584419188240162, -232.5492131852532793 ) ) ;
#310 = DIRECTION ( 'NONE',  ( -6.982962677686266711E-15, 1.000000000000000000, 0.000000000000000000 ) ) ;
#311 = DIRECTION ( 'NONE',  ( -0.1736481776669307198, 2.126576849575776229E-17, 0.9848077530122080203 ) ) ;
#312 = CARTESIAN_POINT ( 'NONE',  ( -13.65925618638770800, 3.289586759644148817, -222.1579143493116533 ) ) ;
#313 = CARTESIAN_POINT ( 'NONE',  ( 8.958604797576050771, -20.52636309154128114, -232.6441826665315205 ) ) ;
#315 = EDGE_CURVE ( 'NONE', #15629, #11616, #21983, .T. ) ;
#314 = PRESENTATION_STYLE_ASSIGNMENT (( #17535 ) ) ;
#316 = CARTESIAN_POINT ( 'NONE',  ( -24.43175472503111223, 5.307112681608126437, 8.481714195412854096 ) ) ;
#317 = CARTESIAN_POINT ( 'NONE',  ( 20.64430047260004031, 12.67811357335941480, -231.0449411089858813 ) ) ;
#318 = CARTESIAN_POINT ( 'NONE',  ( -12.38801939673351704, 9.361418580567464787, -232.8075769614211765 ) ) ;
#319 = CIRCLE ( 'NONE', #11443, 13.12488928717151637 ) ;
#320 = CARTESIAN_POINT ( 'NONE',  ( 0.000000000000000000, -23.00000000000006040, 75.00000000000000000 ) ) ;
#321 = CARTESIAN_POINT ( 'NONE',  ( 11.40028598017942230, 13.60807601628675023, -220.9105305289655519 ) ) ;
#322 = CARTESIAN_POINT ( 'NONE',  ( 2.859576749041432553, -13.55982619688326984, -227.5954719880151345 ) ) ;
#323 = CARTESIAN_POINT ( 'NONE',  ( 22.47485217157460724, -0.5904823501021798648, -216.4383471256914220 ) ) ;
#324 = VERTEX_POINT ( 'NONE', #21527 ) ;
#325 = CARTESIAN_POINT ( 'NONE',  ( -4.784012432433236484, 23.31984772163034947, -232.0554186943449508 ) ) ;
#326 = CARTESIAN_POINT ( 'NONE',  ( -27.32939371162572684, 5.861081283609568260, -224.9659309793921409 ) ) ;
#327 = CARTESIAN_POINT ( 'NONE',  ( -20.76981451797363576, 10.27702766794165257, -234.3988437453480742 ) ) ;
#328 = ORIENTED_EDGE ( 'NONE', *, *, #15715, .F. ) ;
#329 = CARTESIAN_POINT ( 'NONE',  ( -13.78780214743967214, -7.867619234746639378, -226.3818292120506044 ) ) ;
#330 = DIRECTION ( 'NONE',  ( 1.000000000000000000, 0.000000000000000000, 0.000000000000000000 ) ) ;
#331 = EDGE_LOOP ( 'NONE', ( #8318, #981, #21331, #9100 ) ) ;
#332 = CARTESIAN_POINT ( 'NONE',  ( 15.21408433160105034, 3.021350230896802103, -222.3056493717910769 ) ) ;
#333 = CARTESIAN_POINT ( 'NONE',  ( -2.392195434554431177, -23.29395655963766387, -232.4094703796048691 ) ) ;
#334 = CARTESIAN_POINT ( 'NONE',  ( 13.49011766416699842, 7.659170998773840111, -228.1905628957712793 ) ) ;
#335 = CARTESIAN_POINT ( 'NONE',  ( -19.00318367631585659, 13.14621133775862916, -233.8403879275295765 ) ) ;
#336 = AXIS2_PLACEMENT_3D ( 'NONE', #20789, #15968, #7308 ) ;
#337 = CARTESIAN_POINT ( 'NONE',  ( 22.49659352743751128, 7.060662713609715979, -215.7089950799439180 ) ) ;
#338 = CARTESIAN_POINT ( 'NONE',  ( 11.33210854356620523, 22.81476816607802149, -217.8536224460118262 ) ) ;
#339 = CARTESIAN_POINT ( 'NONE',  ( 1.322875655532295358, 1.500000000000000000, -120.0000000000000000 ) ) ;
#340 = CARTESIAN_POINT ( 'NONE',  ( 2.378655016347637652, -14.31292064579845302, -219.9942319014987220 ) ) ;
#341 = CARTESIAN_POINT ( 'NONE',  ( 14.02668320743028119, -5.282748560960272677, -221.9001732195871739 ) ) ;
#342 = CARTESIAN_POINT ( 'NONE',  ( 4.100000000000000533, 0.000000000000000000, -103.0000000000000000 ) ) ;
#343 = DIRECTION ( 'NONE',  ( -1.000000000000000000, 0.000000000000000000, 0.000000000000000000 ) ) ;
#344 = CARTESIAN_POINT ( 'NONE',  ( -22.56222084847001597, 18.89892770556097901, -231.8972396388394088 ) ) ;
#345 = CARTESIAN_POINT ( 'NONE',  ( -21.86011749369748713, -1.271659148212478385, -218.8339345395071689 ) ) ;
#346 = CARTESIAN_POINT ( 'NONE',  ( 18.30177952310522471, 1.918278963380847468, -233.8574151782075887 ) ) ;
#347 = CARTESIAN_POINT ( 'NONE',  ( -1.433739110790628102, 17.19322394474796667, -219.1420620387681879 ) ) ;
#348 = CARTESIAN_POINT ( 'NONE',  ( 5.563568780623874943, 21.86458082533069103, -218.6474243140849012 ) ) ;
#349 = ORIENTED_EDGE ( 'NONE', *, *, #13277, .F. ) ;
#350 = CARTESIAN_POINT ( 'NONE',  ( 16.60513614482655598, -17.51558294309126396, -234.8138649271977556 ) ) ;
#351 = VERTEX_POINT ( 'NONE', #11636 ) ;
#352 = B_SPLINE_CURVE_WITH_KNOTS ( 'NONE', 3,
 ( #8357, #15550, #7861, #19875, #11124, #19133, #17576, #21456, #15667, #18213, #874, #4462, #19250, #14508, #21343, #11230, #7115, #13028, #2035, #4244, #2667, #20932 ),
 .UNSPECIFIED., .F., .F.,
 ( 4, 2, 2, 2, 2, 2, 2, 2, 2, 2, 4 ),
 ( 4.821909171845164511E-17, 0.0003011134387877908666, 0.0006022268775755335946, 0.001204453755151019051, 0.001806680632726504615, 0.002408907510301990396, 0.003011134387877475744, 0.003613361265452961091, 0.004215588143028446873, 0.004516701581816189547, 0.004817815020603932220 ),
 .UNSPECIFIED. ) ;
#353 = CARTESIAN_POINT ( 'NONE',  ( 15.42212722119060864, 5.401662248084913465, -220.8333402320903645 ) ) ;
#354 = CARTESIAN_POINT ( 'NONE',  ( -14.30096418567650041, 6.974026439069829664, -228.7941652905285537 ) ) ;
#355 = CARTESIAN_POINT ( 'NONE',  ( -11.19223248830523332, 8.463078350427430507, -222.6400917074981578 ) ) ;
#356 = CARTESIAN_POINT ( 'NONE',  ( -29.74115761720981510, -1.844952462305729401, -220.6656484738778943 ) ) ;
#357 = EDGE_CURVE ( 'NONE', #14271, #20366, #5815, .T. ) ;
#358 = CARTESIAN_POINT ( 'NONE',  ( -12.90983082593748676, 14.84936372681532823, -233.8009687022269532 ) ) ;
#359 = CARTESIAN_POINT ( 'NONE',  ( 0.000000000000000000, 19.63401512838747820, 77.51594804401857175 ) ) ;
#360 = CARTESIAN_POINT ( 'NONE',  ( 29.55842656951424985, 4.785221541509360854, -220.5134865854112718 ) ) ;
#361 = CARTESIAN_POINT ( 'NONE',  ( -13.06839468023815165, 25.32320678245788059, -229.0099538679170053 ) ) ;
#362 = CARTESIAN_POINT ( 'NONE',  ( 17.65694480011521250, 15.62497337860048674, -235.2008064134603273 ) ) ;
#363 = CARTESIAN_POINT ( 'NONE',  ( -13.93333636822611155, 3.327141996558931947, -221.4468162587888287 ) ) ;
#364 = CARTESIAN_POINT ( 'NONE',  ( -21.94322237485859972, -13.31528874885349900, -215.4027562252440759 ) ) ;
#365 = B_SPLINE_CURVE_WITH_KNOTS ( 'NONE', 3,
 ( #19193, #15943, #12227, #16055, #301, #15724, #3991, #3770, #10538, #17522, #13928, #189, #519, #20763, #5345, #3654, #17407, #7171, #15832, #5457, #14265, #12340 ),
 .UNSPECIFIED., .F., .F.,
 ( 4, 2, 2, 2, 2, 2, 2, 2, 2, 2, 4 ),
 ( 0.4999446919652688059, 0.5028747035357847839, 0.5058047151063008728, 0.5087347266768169618, 0.5116647382473329397, 0.5145947498178489177, 0.5175247613883648956, 0.5204547729588808735, 0.5233847845293969625, 0.5268031313616656774, 0.5278645943380111394 ),
 .UNSPECIFIED. ) ;
#366 = CARTESIAN_POINT ( 'NONE',  ( -29.90835019730369737, -3.078401082523886334, -228.7630230812432046 ) ) ;
#367 = CARTESIAN_POINT ( 'NONE',  ( -19.40752943788874774, 15.61499612050012864, -234.7624367253776541 ) ) ;
#368 = CARTESIAN_POINT ( 'NONE',  ( -5.519971913460887336, -12.21762732219001713, -227.2962593638428359 ) ) ;
#369 = CARTESIAN_POINT ( 'NONE',  ( 8.496844655769807630, 14.66037471857024599, -219.1631158796573118 ) ) ;
#370 = CARTESIAN_POINT ( 'NONE',  ( 12.77158894069672357, -20.43488010613652150, -235.1868042311012914 ) ) ;
#371 = CARTESIAN_POINT ( 'NONE',  ( 0.000000000000000000, -17.50000000000000711, -30.00000000000000000 ) ) ;
#372 = CARTESIAN_POINT ( 'NONE',  ( -16.32047052250102581, 2.570795953410685009, -230.9329235942756213 ) ) ;
#373 = CARTESIAN_POINT ( 'NONE',  ( 1.296323513242173542, 20.09034598902932345, -230.5712631353794961 ) ) ;
#374 = CARTESIAN_POINT ( 'NONE',  ( -16.27882490622757672, 1.520697279646460398, -219.2607721384596289 ) ) ;
#375 = CARTESIAN_POINT ( 'NONE',  ( 24.57222455393806015, 12.08236629421828212, -229.7319216558644541 ) ) ;
#376 = CARTESIAN_POINT ( 'NONE',  ( -22.10934047915427314, 0.9940043559354312386, -216.9999999999999716 ) ) ;
#377 = CARTESIAN_POINT ( 'NONE',  ( -16.08690871037762449, -24.16943144049835368, -222.8355329163958345 ) ) ;
#378 = CARTESIAN_POINT ( 'NONE',  ( 2.276720224425493821, 13.44951395023989171, -229.9230017221896105 ) ) ;
#379 = FACE_OUTER_BOUND ( 'NONE', #20962, .T. ) ;
#380 = CARTESIAN_POINT ( 'NONE',  ( -1.821616882984092411, -20.20372127477041246, -234.2708619787750308 ) ) ;
#381 = CARTESIAN_POINT ( 'NONE',  ( -8.407534899841293097, 16.91942258446019665, -231.3029992963236339 ) ) ;
#382 = CARTESIAN_POINT ( 'NONE',  ( 6.566035546683759883, 15.06745272174450712, -218.8330720708048034 ) ) ;
#383 = CARTESIAN_POINT ( 'NONE',  ( -23.77327857871830830, 11.53128597905896768, -221.0855018166512025 ) ) ;
#384 = CARTESIAN_POINT ( 'NONE',  ( -13.41298582792616934, 27.85383138489214616, -228.6457525465575884 ) ) ;
#385 = CARTESIAN_POINT ( 'NONE',  ( 28.62253243811995418, 3.652502539191337494, -225.4068779441649326 ) ) ;
#386 = EDGE_LOOP ( 'NONE', ( #10513, #13863, #2222, #14894 ) ) ;
#387 = CARTESIAN_POINT ( 'NONE',  ( 6.831421020708281944, -16.86748893536391591, -229.5305077739217552 ) ) ;
#388 = CARTESIAN_POINT ( 'NONE',  ( 11.75796858304313375, -24.75965012883946414, -219.8219186532837455 ) ) ;
#389 = CARTESIAN_POINT ( 'NONE',  ( -9.175187729848801155, 26.50888816229029743, -227.9285554593684253 ) ) ;
#390 = CARTESIAN_POINT ( 'NONE',  ( 25.50000000000000000, -0.5000000000000000000, 0.000000000000000000 ) ) ;
#391 = CARTESIAN_POINT ( 'NONE',  ( 10.85888002857596923, 15.81835858589122878, -232.3913150909872627 ) ) ;
#392 = CARTESIAN_POINT ( 'NONE',  ( 19.63495056682994289, -4.096126682090319271, -232.1271738766904207 ) ) ;
#393 = CARTESIAN_POINT ( 'NONE',  ( -12.44777057840899559, -8.577008958641105352, -229.4809580173677830 ) ) ;
#394 = CARTESIAN_POINT ( 'NONE',  ( 1.729916699924999746, -18.64927252049523432, -233.5000329212076906 ) ) ;
#395 = CARTESIAN_POINT ( 'NONE',  ( -3.139695637132168038, 25.12735071829084177, -230.1469660918596389 ) ) ;
#396 = CARTESIAN_POINT ( 'NONE',  ( 19.31922195716811430, 9.600631919686000160, -218.1359845693048101 ) ) ;
#397 = CARTESIAN_POINT ( 'NONE',  ( -2.772442535524381579, 13.75675912271027457, -228.9770533867650215 ) ) ;
#398 = CARTESIAN_POINT ( 'NONE',  ( -4.285397168228398890, 18.56782363833054106, -219.4990091916804715 ) ) ;
#399 = ORIENTED_EDGE ( 'NONE', *, *, #20384, .T. ) ;
#400 = CARTESIAN_POINT ( 'NONE',  ( 8.860681144154234801, 27.11956268701432293, -229.8503778060109823 ) ) ;
#401 = CARTESIAN_POINT ( 'NONE',  ( 21.96352831578506937, -0.3315607655626218175, -233.9427286327412787 ) ) ;
#402 = CARTESIAN_POINT ( 'NONE',  ( 26.50744623559791435, 1.694095366541529923, -217.6968951254705473 ) ) ;
#403 = CARTESIAN_POINT ( 'NONE',  ( 5.920964624126254350, -19.79845160325395526, -232.2234910544682123 ) ) ;
#404 = CARTESIAN_POINT ( 'NONE',  ( 15.51129552754472307, 0.2180314803830030457, -231.3815478022924879 ) ) ;
#405 = CARTESIAN_POINT ( 'NONE',  ( 25.50000000000000000, -4.400000000000000355, -3.299999999999998490 ) ) ;
#406 = CARTESIAN_POINT ( 'NONE',  ( 4.301648988406530094, 13.23079486486395240, -223.2766268961034655 ) ) ;
#407 = CARTESIAN_POINT ( 'NONE',  ( 19.48258831087540344, -3.612136468958778934, -219.4255404790470436 ) ) ;
#408 = DIRECTION ( 'NONE',  ( 1.000000000000000000, 0.000000000000000000, 0.000000000000000000 ) ) ;
#409 = CARTESIAN_POINT ( 'NONE',  ( 15.52719855059926424, 1.633696074270991172, -221.7349885876216433 ) ) ;
#410 = CARTESIAN_POINT ( 'NONE',  ( 5.569356713096689226, -12.06902110579006226, -223.1407905962607003 ) ) ;
#411 = DIRECTION ( 'NONE',  ( 0.000000000000000000, 0.000000000000000000, 1.000000000000000000 ) ) ;
#412 = CARTESIAN_POINT ( 'NONE',  ( -13.58874046263339608, 12.73011668665171392, -216.5659449791897941 ) ) ;
#413 = CARTESIAN_POINT ( 'NONE',  ( -8.329232059016652201, 11.81357365351366617, -230.1839637212758021 ) ) ;
#414 = ORIENTED_EDGE ( 'NONE', *, *, #15901, .T. ) ;
#415 = CARTESIAN_POINT ( 'NONE',  ( -17.88126539071149779, 5.766250685202066961, -232.9050303536861293 ) ) ;
#416 = CARTESIAN_POINT ( 'NONE',  ( -10.46545893407769157, -9.768586176915025732, -226.8636372813723199 ) ) ;
#417 = CARTESIAN_POINT ( 'NONE',  ( 0.000000000000000000, 25.00000000000000000, 75.00000000000000000 ) ) ;
#418 = CARTESIAN_POINT ( 'NONE',  ( -22.24589463867734906, 5.847797018635430888, 8.118367508314726422 ) ) ;
#419 = CARTESIAN_POINT ( 'NONE',  ( -29.95012366401462955, 4.746560250930182967, -224.6954343660969471 ) ) ;
#420 = CARTESIAN_POINT ( 'NONE',  ( 5.240643865192946116, -17.54789557311951143, -217.3772572127879812 ) ) ;
#421 = DIRECTION ( 'NONE',  ( -0.2588190451025213501, 0.000000000000000000, 0.9659258262890680902 ) ) ;
#422 = CARTESIAN_POINT ( 'NONE',  ( 1.526556658859590748E-13, -21.00000000000006395, -75.00000000000000000 ) ) ;
#423 = CARTESIAN_POINT ( 'NONE',  ( 12.56556766396551872, 9.776144415819011613, -223.4791766911294815 ) ) ;
#424 = CARTESIAN_POINT ( 'NONE',  ( -14.00980274651940682, 20.05588230486321066, -234.2453272803952586 ) ) ;
#425 = CARTESIAN_POINT ( 'NONE',  ( -21.00000000000000000, 0.000000000000000000, 75.00000000000000000 ) ) ;
#426 = CARTESIAN_POINT ( 'NONE',  ( 14.72046356508972309, 21.23077830076469041, -229.4562045376679578 ) ) ;
#427 = CARTESIAN_POINT ( 'NONE',  ( 4.354371064427007276, -19.91633591276652382, -233.4790676556106348 ) ) ;
#428 = ORIENTED_EDGE ( 'NONE', *, *, #5250, .F. ) ;
#429 = CARTESIAN_POINT ( 'NONE',  ( -4.170472558179216804, 16.67407401355319152, -230.2690496885289804 ) ) ;
#430 = CARTESIAN_POINT ( 'NONE',  ( -12.04619960554013502, 10.22290173510000777, -223.1766370265664534 ) ) ;
#431 = CARTESIAN_POINT ( 'NONE',  ( -25.00745438246740804, 14.90779342625281778, -219.2410538611701156 ) ) ;
#432 = CONICAL_SURFACE ( 'NONE', #4015, 25.00000000000001066, 0.2617993877991500740 ) ;
#433 = CARTESIAN_POINT ( 'NONE',  ( -20.58582428111024853, -15.24952116403520463, -229.8418230779359135 ) ) ;
#434 = DIRECTION ( 'NONE',  ( 0.000000000000000000, -1.000000000000000000, 0.000000000000000000 ) ) ;
#435 = ORIENTED_EDGE ( 'NONE', *, *, #10221, .T. ) ;
#436 = CARTESIAN_POINT ( 'NONE',  ( 14.70646826691583975, 6.155951851203820269, -230.2899142379868920 ) ) ;
#437 = CARTESIAN_POINT ( 'NONE',  ( 6.831421020708281944, -16.86748893536391591, -229.5305077739217552 ) ) ;
#438 = CARTESIAN_POINT ( 'NONE',  ( 26.29894631880581812, 12.29609390142961090, -226.3100047295820332 ) ) ;
#439 = CARTESIAN_POINT ( 'NONE',  ( -24.24202834850560606, 19.05981756344202438, -226.6980666352953335 ) ) ;
#440 = EDGE_CURVE ( 'NONE', #17900, #18699, #12299, .T. ) ;
#441 = CARTESIAN_POINT ( 'NONE',  ( 16.77642802340811556, -0.6192566135115280535, -218.8326447441449432 ) ) ;
#442 = CIRCLE ( 'NONE', #19821, 21.63401512838748175 ) ;
#443 = CARTESIAN_POINT ( 'NONE',  ( 4.603870848087811218, 30.13529352683433515, -225.9623629403671430 ) ) ;
#444 = FACE_OUTER_BOUND ( 'NONE', #12908, .T. ) ;
#445 = CARTESIAN_POINT ( 'NONE',  ( -11.07688804854283049, -12.81333559660784971, -232.1241261852632363 ) ) ;
#446 = CARTESIAN_POINT ( 'NONE',  ( 20.25084204406298127, -10.11176871144018818, -232.7817218064674591 ) ) ;
#447 = CARTESIAN_POINT ( 'NONE',  ( 1.526556658859590243E-13, -22.63401512838748175, -77.51594804401857175 ) ) ;
#448 = LINE ( 'NONE', #14302, #21639 ) ;
#449 = CARTESIAN_POINT ( 'NONE',  ( -18.67456582549428390, 11.07053394491094345, -214.7114755712704550 ) ) ;
#450 = CARTESIAN_POINT ( 'NONE',  ( -16.09675311661892039, -3.241155435977624677, -226.6155721728984531 ) ) ;
#451 = CARTESIAN_POINT ( 'NONE',  ( -17.39737143130126285, 7.531548707695031375, -232.0788227848755696 ) ) ;
#452 = CARTESIAN_POINT ( 'NONE',  ( 3.219568897812384645, 28.82511222849302257, -221.5626884747494216 ) ) ;
#453 = CARTESIAN_POINT ( 'NONE',  ( -2.125813515909480866, 15.68152656492264363, -220.3943115937447317 ) ) ;
#454 = ORIENTED_EDGE ( 'NONE', *, *, #861, .T. ) ;
#455 = CARTESIAN_POINT ( 'NONE',  ( 20.57969228301723419, -8.207465571703625784, -214.6085555290863454 ) ) ;
#456 = ORIENTED_EDGE ( 'NONE', *, *, #16713, .T. ) ;
#457 = CARTESIAN_POINT ( 'NONE',  ( 28.02123297569005089, 5.903198806000402143, -227.5759114383273811 ) ) ;
#458 = CIRCLE ( 'NONE', #800, 23.00000000000000000 ) ;
#459 = CARTESIAN_POINT ( 'NONE',  ( -12.39195900010699702, 23.13258866008456138, -233.4668451572263166 ) ) ;
#460 = CARTESIAN_POINT ( 'NONE',  ( -15.10760069511485604, 3.026516874529453283, -224.5685390982118861 ) ) ;
#461 = CARTESIAN_POINT ( 'NONE',  ( -15.34124043857492303, -4.213426711746545372, -218.8308339851419078 ) ) ;
#462 = CARTESIAN_POINT ( 'NONE',  ( -19.25929423112888017, 9.818144317380269825, -216.1837936240308409 ) ) ;
#463 = CARTESIAN_POINT ( 'NONE',  ( 1.526556658859590243E-13, -22.63401512838748175, 77.51594804401857175 ) ) ;
#464 = EDGE_CURVE ( 'NONE', #19761, #19544, #19810, .T. ) ;
#465 = CARTESIAN_POINT ( 'NONE',  ( 23.21336156720804667, 12.57464006230432574, -232.9346648124233070 ) ) ;
#466 = CARTESIAN_POINT ( 'NONE',  ( -13.01542355754912172, 26.77630951171455820, -225.1545229496516356 ) ) ;
#467 = CARTESIAN_POINT ( 'NONE',  ( 11.17228388010293649, 5.622653638471959425, -222.3672781564363845 ) ) ;
#468 = CARTESIAN_POINT ( 'NONE',  ( -21.89065952084848021, -0.9940043559354364566, -216.9999999999999716 ) ) ;
#469 = CONICAL_SURFACE ( 'NONE', #7660, 23.06814834742187514, 0.2617993877991500740 ) ;
#470 = CARTESIAN_POINT ( 'NONE',  ( -19.24125987773642166, -8.201885216777814236, -235.2928755229699789 ) ) ;
#471 = AXIS2_PLACEMENT_3D ( 'NONE', #20639, #5224, #4585 ) ;
#472 = CARTESIAN_POINT ( 'NONE',  ( -19.29805292978571885, -8.785194383212417080, -233.3520286081516133 ) ) ;
#473 = EDGE_CURVE ( 'NONE', #16430, #17437, #6541, .T. ) ;
#474 = CARTESIAN_POINT ( 'NONE',  ( -1.973648319964989462, 15.33498294326524203, -220.9958390492969329 ) ) ;
#475 = CARTESIAN_POINT ( 'NONE',  ( -7.460068573003235670, -29.58770008691625364, -228.1902472473001637 ) ) ;
#476 = CARTESIAN_POINT ( 'NONE',  ( 4.484811161826725900, 15.38298568785217313, -219.4617573400562662 ) ) ;
#477 = CARTESIAN_POINT ( 'NONE',  ( 3.668385877085885927, -11.51845067838601366, -222.7629028536941291 ) ) ;
#478 = CARTESIAN_POINT ( 'NONE',  ( 0.000000000000000000, 0.000000000000000000, 69.99999999999998579 ) ) ;
#479 = CARTESIAN_POINT ( 'NONE',  ( 29.47107563651793427, 6.731311671946880182, -220.0565342412898815 ) ) ;
#480 = CARTESIAN_POINT ( 'NONE',  ( 30.39189047201120175, -1.943849802383817993, -228.0804048816970919 ) ) ;
#481 = CARTESIAN_POINT ( 'NONE',  ( -4.285397168228398890, 18.56782363833054106, -219.4990091916804715 ) ) ;
#482 = CARTESIAN_POINT ( 'NONE',  ( 17.34461553379066601, 6.893916422670210764, -233.3442385185644525 ) ) ;
#483 = CARTESIAN_POINT ( 'NONE',  ( 24.42567939027770407, 10.22651298688739097, -219.4562066833365748 ) ) ;
#484 = CARTESIAN_POINT ( 'NONE',  ( -13.44952714103469305, -17.53057434768947331, -217.9956016333683237 ) ) ;
#485 = EDGE_CURVE ( 'NONE', #10116, #8679, #18757, .T. ) ;
#486 = CARTESIAN_POINT ( 'NONE',  ( 1.220475224794998370, 29.83033731899746144, -230.4224274340063801 ) ) ;
#487 = AXIS2_PLACEMENT_3D ( 'NONE', #4624, #8133, #8020 ) ;
#488 = CIRCLE ( 'NONE', #9121, 3.000000000000002665 ) ;
#489 = CARTESIAN_POINT ( 'NONE',  ( 0.000000000000000000, 0.000000000000000000, 75.01817430661621700 ) ) ;
#490 = CARTESIAN_POINT ( 'NONE',  ( -3.608027314846280031, -12.96557536209330763, -219.9492366723279702 ) ) ;
#491 = CARTESIAN_POINT ( 'NONE',  ( -7.240690404266621805, 13.01623002570985044, -225.3000933658701967 ) ) ;
#492 = CARTESIAN_POINT ( 'NONE',  ( 23.22505041959077232, 19.39625294115234055, -221.5972645870541555 ) ) ;
#493 = CARTESIAN_POINT ( 'NONE',  ( -11.82020046940938407, 10.16362659047642758, -224.3364193436540575 ) ) ;
#494 = CARTESIAN_POINT ( 'NONE',  ( -3.309130212696198559, 28.80211350556483296, -217.4284252357080334 ) ) ;
#495 = CARTESIAN_POINT ( 'NONE',  ( 14.70646826691583975, 6.155951851203820269, -230.2899142379868920 ) ) ;
#496 = CARTESIAN_POINT ( 'NONE',  ( 11.33829581046623858, -17.80819325066959635, -230.7883484307220385 ) ) ;
#497 = VERTEX_POINT ( 'NONE', #16816 ) ;
#498 = CARTESIAN_POINT ( 'NONE',  ( 11.72194121175188997, -15.95900783718691507, -217.6519982781775013 ) ) ;
#499 = CARTESIAN_POINT ( 'NONE',  ( -6.901278853520646628, 15.41233971300566807, -220.5972764307651346 ) ) ;
#500 = CARTESIAN_POINT ( 'NONE',  ( -17.50000000000001066, 2.143131898507869431E-15, -30.00000000000000000 ) ) ;
#501 = CARTESIAN_POINT ( 'NONE',  ( 17.60676319847677007, 21.31475060840986302, -219.8266339603936785 ) ) ;
#502 = CARTESIAN_POINT ( 'NONE',  ( 24.56541673123750158, -5.996287403333383281, -231.6940117905984664 ) ) ;
#503 = CARTESIAN_POINT ( 'NONE',  ( -15.22366728182010043, -5.552021002219007961, -230.2511309519622671 ) ) ;
#504 = CARTESIAN_POINT ( 'NONE',  ( -7.800954605602409053, -29.95157606033723496, -226.5906573908930000 ) ) ;
#505 = CARTESIAN_POINT ( 'NONE',  ( -5.125319492185865577, 20.53749879880200524, -218.7557759432853288 ) ) ;
#506 = CARTESIAN_POINT ( 'NONE',  ( 22.56777165119825668, 0.000000000000000000, 90.00000000000000000 ) ) ;
#507 = CARTESIAN_POINT ( 'NONE',  ( 20.22510869507564024, 17.05975164568011238, -220.7829296213589316 ) ) ;
#508 = CARTESIAN_POINT ( 'NONE',  ( -17.75316132689678383, 25.03468689048078843, -222.1645193425721061 ) ) ;
#509 = CARTESIAN_POINT ( 'NONE',  ( -9.115411286166651195, 13.66191091052436235, -230.3338332872444312 ) ) ;
#510 = ORIENTED_EDGE ( 'NONE', *, *, #7205, .T. ) ;
#511 = CARTESIAN_POINT ( 'NONE',  ( 6.040050017043670394, 13.67534390435379699, -220.4759402345340504 ) ) ;
#512 = CARTESIAN_POINT ( 'NONE',  ( -23.67953786836281083, 9.946055673977088674, -229.5560005648173671 ) ) ;
#513 = CARTESIAN_POINT ( 'NONE',  ( 20.64287812348744566, 0.2024751443801864337, -216.7518974727033481 ) ) ;
#514 = CARTESIAN_POINT ( 'NONE',  ( 15.69671663880151868, -19.77919342852767315, -217.9503656454650411 ) ) ;
#515 = LINE ( 'NONE', #19075, #11094 ) ;
#516 = ORIENTED_EDGE ( 'NONE', *, *, #704, .F. ) ;
#517 = CARTESIAN_POINT ( 'NONE',  ( 5.331555957413248059, 27.50712867803999728, -219.0801070358024276 ) ) ;
#518 = CARTESIAN_POINT ( 'NONE',  ( 24.34559900986324621, -8.951716371391148286, -220.6604487471163623 ) ) ;
#519 = CARTESIAN_POINT ( 'NONE',  ( 25.54997870115619207, -2.097555195297153841, -218.7002440566220400 ) ) ;
#520 = CARTESIAN_POINT ( 'NONE',  ( 4.201723131641114328, -20.76291977712905279, -215.9522215885928347 ) ) ;
#521 = CARTESIAN_POINT ( 'NONE',  ( -22.17339560624464312, 16.26550580028390769, -232.0582861498566274 ) ) ;
#522 = AXIS2_PLACEMENT_3D ( 'NONE', #21767, #13572, #13228 ) ;
#523 = CARTESIAN_POINT ( 'NONE',  ( -11.40916210110096962, 20.01996232974788725, -234.3205435716851923 ) ) ;
#524 = CARTESIAN_POINT ( 'NONE',  ( -9.443239614166923701, 9.388015667058336788, -222.3195230688234290 ) ) ;
#525 = CARTESIAN_POINT ( 'NONE',  ( -24.95227886253013239, -16.82584358170602101, -223.8363818545792299 ) ) ;
#526 = LINE ( 'NONE', #7615, #8756 ) ;
#527 = CARTESIAN_POINT ( 'NONE',  ( 0.000000000000000000, 0.000000000000000000, 93.00000000000000000 ) ) ;
#528 = CARTESIAN_POINT ( 'NONE',  ( -15.48255455842386219, 10.01793346089237069, -233.1197357361336913 ) ) ;
#529 = CARTESIAN_POINT ( 'NONE',  ( -0.3008257096753846893, -14.77709807386645480, -230.6673697011181048 ) ) ;
#530 = SURFACE_SIDE_STYLE ('',( #12575 ) ) ;
#531 = CARTESIAN_POINT ( 'NONE',  ( 17.24423567610276109, 8.542587572837451404, -218.6562240232607621 ) ) ;
#532 = CARTESIAN_POINT ( 'NONE',  ( -8.894613172508529786, 25.42460746921206294, -232.3150764041658363 ) ) ;
#533 = CARTESIAN_POINT ( 'NONE',  ( 13.70753084697862612, 0.1061737631881888994, -227.9987150399367408 ) ) ;
#534 = CARTESIAN_POINT ( 'NONE',  ( 10.64724148863252395, 12.28344647332184181, -223.6549461381946173 ) ) ;
#535 = CARTESIAN_POINT ( 'NONE',  ( 2.980115756258533644, -14.12936798750240008, -229.0659090661425807 ) ) ;
#536 = EDGE_LOOP ( 'NONE', ( #20404, #210, #5432, #5454, #20475, #13502 ) ) ;
#537 = CARTESIAN_POINT ( 'NONE',  ( -8.857704405076667342, 24.20848540845601704, -218.8859504303524091 ) ) ;
#538 = CARTESIAN_POINT ( 'NONE',  ( -13.06839468023815165, 25.32320678245788059, -229.0099538679170053 ) ) ;
#539 = CARTESIAN_POINT ( 'NONE',  ( -27.12694304224540076, 7.756125161462346540, -217.3817363082233101 ) ) ;
#540 = AXIS2_PLACEMENT_3D ( 'NONE', #11823, #9916, #17115 ) ;
#541 = CARTESIAN_POINT ( 'NONE',  ( -14.65844530258765310, -17.20867344037294444, -230.8340913472024170 ) ) ;
#542 = CARTESIAN_POINT ( 'NONE',  ( 1.665334536937735820E-13, -23.00000000000006040, 69.99999999999998579 ) ) ;
#543 = ORIENTED_EDGE ( 'NONE', *, *, #7416, .T. ) ;
#544 = PRESENTATION_LAYER_ASSIGNMENT (  '', '', ( #18518 ) ) ;
#545 = CARTESIAN_POINT ( 'NONE',  ( -25.29098058636142810, 5.014641116111857144, -217.4658967307323110 ) ) ;
#546 = CARTESIAN_POINT ( 'NONE',  ( 8.290903921942224031, -23.90349455650518351, -230.1727405421096364 ) ) ;
#547 = CARTESIAN_POINT ( 'NONE',  ( 10.78187269046063435, 10.73871010366167944, -221.9206544238666368 ) ) ;
#548 = CARTESIAN_POINT ( 'NONE',  ( -8.501641725227710111, 25.47064987787527102, -217.3358698761548737 ) ) ;
#549 = CARTESIAN_POINT ( 'NONE',  ( -15.60078324628501356, 3.527872497691606934, -227.4630248446626695 ) ) ;
#550 = EDGE_CURVE ( 'NONE', #16938, #19932, #17685, .T. ) ;
#551 = CARTESIAN_POINT ( 'NONE',  ( 4.484811161826725900, 15.38298568785217313, -219.4617573400562662 ) ) ;
#552 = CARTESIAN_POINT ( 'NONE',  ( -10.76794919243112325, -2.704190363445815236E-15, 92.00000000000000000 ) ) ;
#553 = AXIS2_PLACEMENT_3D ( 'NONE', #16638, #4473, #5947 ) ;
#554 = CARTESIAN_POINT ( 'NONE',  ( -15.62091161899253855, -26.00636881980398840, -222.1463585103649905 ) ) ;
#555 = PRESENTATION_LAYER_ASSIGNMENT (  '', '', ( #17096 ) ) ;
#556 = CARTESIAN_POINT ( 'NONE',  ( 17.28140336138120858, -11.48510652344925020, -216.9852223368602893 ) ) ;
#557 = DIRECTION ( 'NONE',  ( 0.000000000000000000, 0.000000000000000000, -1.000000000000000000 ) ) ;
#558 = DIRECTION ( 'NONE',  ( -0.000000000000000000, -1.000000000000000000, -0.000000000000000000 ) ) ;
#559 = CARTESIAN_POINT ( 'NONE',  ( -14.08083899843152231, 10.81596681319144970, -234.3239311387574446 ) ) ;
#560 = CARTESIAN_POINT ( 'NONE',  ( -27.33303184979533285, -3.055344081261842870, -227.4850045670461043 ) ) ;
#561 = CARTESIAN_POINT ( 'NONE',  ( -13.31590776630363315, 5.340120742929252096, -225.6956515496373186 ) ) ;
#562 = CARTESIAN_POINT ( 'NONE',  ( 8.379126514044342500, 15.76264856365358646, -232.1787896114811360 ) ) ;
#563 = CARTESIAN_POINT ( 'NONE',  ( -1.238249567024760189, 29.30580384236933966, -223.2399636023643836 ) ) ;
#564 = ORIENTED_EDGE ( 'NONE', *, *, #4047, .T. ) ;
#565 = CARTESIAN_POINT ( 'NONE',  ( 19.43707201973751708, -21.22621598813149646, -232.3303264720597667 ) ) ;
#566 = VERTEX_POINT ( 'NONE', #2846 ) ;
#567 = CARTESIAN_POINT ( 'NONE',  ( 18.46552355142154411, 5.019711608606525211, -231.5099115070375433 ) ) ;
#568 = CARTESIAN_POINT ( 'NONE',  ( -4.531689447889125866, 14.11317536318881416, -231.6806015375303502 ) ) ;
#569 = CARTESIAN_POINT ( 'NONE',  ( -6.111257124579617894, 15.89946952501658295, -216.3497764690875727 ) ) ;
#570 = CARTESIAN_POINT ( 'NONE',  ( -14.31049420963804586, -8.435107166214018903, -218.7432863707801403 ) ) ;
#571 = CARTESIAN_POINT ( 'NONE',  ( -9.171998067665157350, 9.395241133357435714, -226.3428046914542051 ) ) ;
#572 = LINE ( 'NONE', #18015, #14095 ) ;
#573 = PRESENTATION_LAYER_ASSIGNMENT (  '', '', ( #14611 ) ) ;
#574 = DIRECTION ( 'NONE',  ( -1.000000000000000000, 0.000000000000000000, 0.000000000000000000 ) ) ;
#575 = CARTESIAN_POINT ( 'NONE',  ( -12.96364545172611571, 10.77137376900670063, -221.1208843751685720 ) ) ;
#576 = CARTESIAN_POINT ( 'NONE',  ( -19.50431861204945605, -0.7624880359591150736, -219.4666829195064395 ) ) ;
#577 = CARTESIAN_POINT ( 'NONE',  ( -14.87984907657228639, 0.2138881189739126887, -228.7773920408832282 ) ) ;
#578 = CARTESIAN_POINT ( 'NONE',  ( 7.995304978256253747, 13.28024228361502779, -220.6535174700288451 ) ) ;
#579 = CARTESIAN_POINT ( 'NONE',  ( -24.09642229725868745, -17.04339013636034750, -228.1169379854252384 ) ) ;
#580 = VERTEX_POINT ( 'NONE', #8267 ) ;
#581 = CARTESIAN_POINT ( 'NONE',  ( -6.072587425033909803, 24.65158735603439055, -217.4249768037189767 ) ) ;
#582 = CARTESIAN_POINT ( 'NONE',  ( -5.636842872076440081, -13.76003991320737541, -219.7405193562604495 ) ) ;
#583 = CARTESIAN_POINT ( 'NONE',  ( 16.54345861550681107, 19.37554510112122230, -218.2240151908141002 ) ) ;
#584 = CARTESIAN_POINT ( 'NONE',  ( 6.919598145955467849, -31.16410449029495311, -226.5345828574877487 ) ) ;
#585 = CARTESIAN_POINT ( 'NONE',  ( 0.000000000000000000, 0.000000000000000000, 75.00000000000000000 ) ) ;
#586 = EDGE_CURVE ( 'NONE', #10093, #20645, #8701, .T. ) ;
#587 = CARTESIAN_POINT ( 'NONE',  ( -9.954421844142357756, 11.21484508112568079, -226.0177122452137439 ) ) ;
#588 = DIRECTION ( 'NONE',  ( 0.000000000000000000, 0.000000000000000000, -1.000000000000000000 ) ) ;
#589 = CARTESIAN_POINT ( 'NONE',  ( 21.96352831578812115, -0.3315607655626495731, -233.9427286327413356 ) ) ;
#590 = CARTESIAN_POINT ( 'NONE',  ( 13.50603691942335693, 22.79443449215731832, -229.7689193854997995 ) ) ;
#591 = CARTESIAN_POINT ( 'NONE',  ( -12.33203608746942237, 8.428128317385924717, -222.9277009507565026 ) ) ;
#592 = CARTESIAN_POINT ( 'NONE',  ( 21.31262902390056624, 0.4111834581965390645, -232.0572713672585792 ) ) ;
#593 = CARTESIAN_POINT ( 'NONE',  ( -9.981957700435337699, -28.23530775694580441, -222.3321348641582347 ) ) ;
#594 = CARTESIAN_POINT ( 'NONE',  ( 13.70863938672594529, 6.616599615120571265, -232.1343637516268643 ) ) ;
#595 = DIRECTION ( 'NONE',  ( 0.000000000000000000, 0.000000000000000000, 1.000000000000000000 ) ) ;
#596 = CARTESIAN_POINT ( 'NONE',  ( 0.4504461526642338232, -19.62726417856956473, -215.9916429883993487 ) ) ;
#597 = CARTESIAN_POINT ( 'NONE',  ( 2.893760225568064115, 14.39521026618305477, -227.6654023557511550 ) ) ;
#598 = EDGE_CURVE ( 'NONE', #15940, #3862, #788, .T. ) ;
#599 = CARTESIAN_POINT ( 'NONE',  ( 14.69853173970351179, 23.44775873627089524, -231.2711109634281001 ) ) ;
#600 = CARTESIAN_POINT ( 'NONE',  ( -8.892156391762910062, 11.89593067802204551, -225.4519868197583889 ) ) ;
#601 = CARTESIAN_POINT ( 'NONE',  ( -4.154119475380428916, 11.54776298361823095, -227.0876712548254943 ) ) ;
#602 = CARTESIAN_POINT ( 'NONE',  ( 15.28706223449149348, 2.473424253736659306, -227.9634568993954531 ) ) ;
#603 = CARTESIAN_POINT ( 'NONE',  ( 9.097575839043912538, -18.13002900832716335, -219.2719510042808224 ) ) ;
#604 = ORIENTED_EDGE ( 'NONE', *, *, #18360, .F. ) ;
#605 = CARTESIAN_POINT ( 'NONE',  ( 13.17817051516727922, -26.22376201054615308, -223.3126545406654486 ) ) ;
#606 = CARTESIAN_POINT ( 'NONE',  ( -6.769588938507062004, 18.22485903270490937, -231.3660928915624879 ) ) ;
#607 = DIRECTION ( 'NONE',  ( -0.000000000000000000, -0.000000000000000000, 1.000000000000000000 ) ) ;
#608 = CARTESIAN_POINT ( 'NONE',  ( 27.04607490430786854, 4.607450003618843049, -220.3758934308003461 ) ) ;
#609 = CARTESIAN_POINT ( 'NONE',  ( 28.52058947142581502, -1.755848367977142610, -221.9695116608532715 ) ) ;
#610 = CARTESIAN_POINT ( 'NONE',  ( -20.11874861854083463, -21.11755179634840474, -229.7504124090357323 ) ) ;
#611 = CARTESIAN_POINT ( 'NONE',  ( 1.623338700557370951, -21.82196275546919040, -234.1129525514646730 ) ) ;
#612 = CARTESIAN_POINT ( 'NONE',  ( 8.829458998963966465, 22.90677303676718779, -219.2026791561175685 ) ) ;
#613 = CARTESIAN_POINT ( 'NONE',  ( -19.79999999999999716, 0.000000000000000000, -78.50000000000000000 ) ) ;
#614 = CARTESIAN_POINT ( 'NONE',  ( -28.99982533490676317, 5.894721259135065949, -231.5937499788843468 ) ) ;
#615 = CARTESIAN_POINT ( 'NONE',  ( -3.643097910890548796, 22.16888955197135047, -233.9701981029593298 ) ) ;
#616 = CARTESIAN_POINT ( 'NONE',  ( 4.044213993247089967, 16.45246633354041421, -227.9255899743332918 ) ) ;
#617 = CARTESIAN_POINT ( 'NONE',  ( -2.692720963948733282, 24.67937284847025481, -218.0912907784291406 ) ) ;
#618 = CARTESIAN_POINT ( 'NONE',  ( -12.04619960554013502, 10.22290173510000777, -223.1766370265664534 ) ) ;
#619 = CARTESIAN_POINT ( 'NONE',  ( 14.17826651990317188, -1.167225063855702683, -222.4240311848849387 ) ) ;
#620 = CARTESIAN_POINT ( 'NONE',  ( 7.045253012492558753, -17.38872841331140862, -218.3726031779064556 ) ) ;
#621 = B_SPLINE_CURVE_WITH_KNOTS ( 'NONE', 3,
 ( #8461, #18585, #1249, #11827, #16893, #8123, #21829, #13288, #15329, #18471, #10030, #3033, #3147, #1359, #8232, #15102, #1467, #8343, #15214, #6763, #13633, #22059 ),
 .UNSPECIFIED., .F., .F.,
 ( 4, 2, 2, 2, 2, 2, 2, 2, 2, 2, 4 ),
 ( 0.005800309973860217315, 0.006162931802046735415, 0.006525553630233253515, 0.006888175458419771614, 0.007250797286606289714, 0.007976040942979321577, 0.008701284599352352572, 0.01015177191209841456, 0.01087701556847144729, 0.01123963739665796366, 0.01160225922484448176 ),
 .UNSPECIFIED. ) ;
#622 = FACE_OUTER_BOUND ( 'NONE', #10894, .T. ) ;
#623 = EDGE_LOOP ( 'NONE', ( #16790, #6594, #15513, #3933, #16241, #20562 ) ) ;
#624 = CARTESIAN_POINT ( 'NONE',  ( 4.543450689403089271, 15.91052110650461771, -218.9437823786444426 ) ) ;
#625 = CARTESIAN_POINT ( 'NONE',  ( -25.88730550323791491, -2.172607277783750845, -234.4881349215252726 ) ) ;
#626 = CARTESIAN_POINT ( 'NONE',  ( 0.000000000000000000, 0.000000000000000000, 94.00000000000000000 ) ) ;
#627 = EDGE_CURVE ( 'NONE', #17378, #2791, #3286, .T. ) ;
#628 = CARTESIAN_POINT ( 'NONE',  ( 8.021672912688133650, -23.92397517040199872, -233.3380040120402441 ) ) ;
#629 = APPLICATION_PROTOCOL_DEFINITION ( 'draft international standard', 'automotive_design', 1998, #6851 ) ;
#630 = CARTESIAN_POINT ( 'NONE',  ( -21.02719846458807851, 18.12262440796364871, -218.0220709499931502 ) ) ;
#631 = CARTESIAN_POINT ( 'NONE',  ( -11.59874896804548250, 27.28969409813203484, -218.8626241359735332 ) ) ;
#632 = ORIENTED_EDGE ( 'NONE', *, *, #6211, .T. ) ;
#633 = CARTESIAN_POINT ( 'NONE',  ( -14.00380962569832199, 8.747390586476997854, -231.7950903513155936 ) ) ;
#634 = CARTESIAN_POINT ( 'NONE',  ( -15.95714424191699266, -19.90201571590360885, -231.7641511196865451 ) ) ;
#635 = DIRECTION ( 'NONE',  ( -0.000000000000000000, -1.000000000000000000, -0.000000000000000000 ) ) ;
#636 = CARTESIAN_POINT ( 'NONE',  ( -21.73616590321354280, 7.534719468122247577, -6.606834546510540029 ) ) ;
#637 = CARTESIAN_POINT ( 'NONE',  ( -18.09776816382430908, 23.50806826204562583, -229.9568677523880638 ) ) ;
#638 = CARTESIAN_POINT ( 'NONE',  ( 9.923594862512629788, -27.47695806889172943, -228.4416101659923015 ) ) ;
#639 = CARTESIAN_POINT ( 'NONE',  ( -11.49049084071896409, 11.06834963248926940, -218.3354249205727058 ) ) ;
#640 = CARTESIAN_POINT ( 'NONE',  ( 18.30590144060498403, 15.06309558287673767, -219.0459394567220102 ) ) ;
#641 = CARTESIAN_POINT ( 'NONE',  ( 5.711092584709906106, 26.13380667269736790, -220.5232813324456629 ) ) ;
#642 = CARTESIAN_POINT ( 'NONE',  ( 0.000000000000000000, 17.50000000000000711, -60.00000000000000000 ) ) ;
#643 = CARTESIAN_POINT ( 'NONE',  ( 24.38255093784924199, 7.851200578213498815, -231.2687759850219607 ) ) ;
#644 = CARTESIAN_POINT ( 'NONE',  ( -11.82770121052164924, -14.33821066513346487, -229.8071374592849452 ) ) ;
#645 = VERTEX_POINT ( 'NONE', #952 ) ;
#646 = CARTESIAN_POINT ( 'NONE',  ( -3.996294969088721505, 28.80481464818193515, -222.8623509149411746 ) ) ;
#647 = CARTESIAN_POINT ( 'NONE',  ( -20.29166677327761903, 16.18344358422343632, -220.0060062064338524 ) ) ;
#648 = CARTESIAN_POINT ( 'NONE',  ( -8.548213857283494477, 12.07277636836182211, -222.5354997492170241 ) ) ;
#649 = CARTESIAN_POINT ( 'NONE',  ( -17.67448836398429890, -11.08962652971676199, -218.7915233441472367 ) ) ;
#650 = DIRECTION ( 'NONE',  ( 1.000000000000000000, 0.000000000000000000, 0.000000000000000000 ) ) ;
#651 = ORIENTED_EDGE ( 'NONE', *, *, #13199, .F. ) ;
#652 = CARTESIAN_POINT ( 'NONE',  ( -28.17543631911187063, 3.557555778861649642, -230.1980773687482156 ) ) ;
#653 = CARTESIAN_POINT ( 'NONE',  ( 0.1655890855189643129, -14.86936674525315993, -225.9040401458518943 ) ) ;
#654 = CARTESIAN_POINT ( 'NONE',  ( 18.76922974182421555, 13.12635134380198210, -217.8010375391909008 ) ) ;
#655 = CARTESIAN_POINT ( 'NONE',  ( -2.817219543927646175, 14.13981714106644993, -229.6779615865167443 ) ) ;
#656 = PRODUCT_DEFINITION_CONTEXT ( 'detailed design', #16058, 'design' ) ;
#657 = CARTESIAN_POINT ( 'NONE',  ( -26.91858181626453472, 10.72837452931393187, -223.4556356000267670 ) ) ;
#658 = CARTESIAN_POINT ( 'NONE',  ( 12.65306858828212810, 29.42930486385247590, -226.3758484992818012 ) ) ;
#659 = CARTESIAN_POINT ( 'NONE',  ( 16.84848658399567611, 11.39632653812981644, -217.9589513831453473 ) ) ;
#660 = AXIS2_PLACEMENT_3D ( 'NONE', #18313, #757, #9432 ) ;
#661 = CARTESIAN_POINT ( 'NONE',  ( 14.83698775855651952, 1.948536915275967507, -222.7182371053496865 ) ) ;
#662 = CARTESIAN_POINT ( 'NONE',  ( -18.64257584594551531, -16.66392856591270899, -217.1407738418131999 ) ) ;
#663 = CARTESIAN_POINT ( 'NONE',  ( 2.967317674205219191, -16.40215926535219282, -217.6245344443522924 ) ) ;
#664 = DIRECTION ( 'NONE',  ( 0.000000000000000000, 0.000000000000000000, -1.000000000000000000 ) ) ;
#665 = DIRECTION ( 'NONE',  ( -0.000000000000000000, -0.000000000000000000, -1.000000000000000000 ) ) ;
#666 = CARTESIAN_POINT ( 'NONE',  ( -7.352050649209116884, 10.05454564170545417, -223.7370967983176229 ) ) ;
#667 = CARTESIAN_POINT ( 'NONE',  ( -26.02538399328502905, -8.003917019953526335, -222.3553134616452098 ) ) ;
#668 = CARTESIAN_POINT ( 'NONE',  ( -14.35594238341465889, 9.236863657925704629, -219.6542735655305307 ) ) ;
#669 = CARTESIAN_POINT ( 'NONE',  ( 23.18902850759750933, 20.27908137164207147, -226.2847847834817117 ) ) ;
#670 = CARTESIAN_POINT ( 'NONE',  ( 10.73846460100926592, 12.62787417135106161, -222.6344468496098159 ) ) ;
#671 = ORIENTED_EDGE ( 'NONE', *, *, #17680, .T. ) ;
#672 = CARTESIAN_POINT ( 'NONE',  ( 18.85502272441424765, -23.46047257272994102, -219.5236553823413317 ) ) ;
#673 = CARTESIAN_POINT ( 'NONE',  ( 16.38151749656409351, 8.902090001712490874, -231.2955017965201989 ) ) ;
#674 = CARTESIAN_POINT ( 'NONE',  ( -13.41298582792616934, 27.85383138489214616, -228.6457525465575884 ) ) ;
#675 = ADVANCED_FACE ( 'NONE', ( #14692 ), #2927, .F. ) ;
#676 = CARTESIAN_POINT ( 'NONE',  ( -4.155456637169709921, 11.30291311430030987, -225.2606024264729001 ) ) ;
#677 = CARTESIAN_POINT ( 'NONE',  ( -22.73457989858237127, -6.881456255901889030, -216.4806380023168799 ) ) ;
#678 = CARTESIAN_POINT ( 'NONE',  ( -10.30050448363967419, 10.07750059423401190, -220.1837019037183723 ) ) ;
#679 = AXIS2_PLACEMENT_3D ( 'NONE', #6039, #12809, #19760 ) ;
#680 = CARTESIAN_POINT ( 'NONE',  ( -1.701984465643862965, -14.42982486328545377, 93.00000000000000000 ) ) ;
#681 = CARTESIAN_POINT ( 'NONE',  ( 24.21331552874348958, 0.07051084380047288602, -231.7986140076958463 ) ) ;
#682 = CARTESIAN_POINT ( 'NONE',  ( -6.804439720554941395, 15.25609613835249156, -218.7834354895107651 ) ) ;
#683 = CARTESIAN_POINT ( 'NONE',  ( 17.96045420455031305, -0.3746358454349600908, -217.9627609769914613 ) ) ;
#684 = CARTESIAN_POINT ( 'NONE',  ( -23.98802705797876200, 19.46654170242919690, -223.5293093576406989 ) ) ;
#685 = CARTESIAN_POINT ( 'NONE',  ( 6.093530912645064745, 16.79941505724243811, -232.1766444656230419 ) ) ;
#686 = DIRECTION ( 'NONE',  ( -0.000000000000000000, -0.000000000000000000, -1.000000000000000000 ) ) ;
#687 = CARTESIAN_POINT ( 'NONE',  ( 0.3355639943343493026, 23.87279439325363128, -218.0067922387550823 ) ) ;
#688 = CARTESIAN_POINT ( 'NONE',  ( -25.61235545225478560, -15.41032726095661509, -226.9890212492312855 ) ) ;
#689 = CARTESIAN_POINT ( 'NONE',  ( 11.67669251569587985, 24.04736029062789981, -218.5856804285192254 ) ) ;
#690 = CARTESIAN_POINT ( 'NONE',  ( 8.343550503364536297, -10.95302570107183726, -218.8523668966870446 ) ) ;
#691 = DIRECTION ( 'NONE',  ( -2.891205793294678696E-17, 0.000000000000000000, -1.000000000000000000 ) ) ;
#692 = CARTESIAN_POINT ( 'NONE',  ( -20.97727766418175932, 9.381545086430262970, -232.5968905491617420 ) ) ;
#693 = CARTESIAN_POINT ( 'NONE',  ( -22.63401512838757057, 0.000000000000000000, -77.51594804401857175 ) ) ;
#694 = CARTESIAN_POINT ( 'NONE',  ( -17.19162585816985001, -4.675655174483583032, -230.6997921109560821 ) ) ;
#695 = CARTESIAN_POINT ( 'NONE',  ( 14.02816775221371337, 20.58276248714641810, -218.7180790146936999 ) ) ;
#696 = CARTESIAN_POINT ( 'NONE',  ( -22.38347148959098121, 12.58966534755613687, -218.4978713241202399 ) ) ;
#697 = CARTESIAN_POINT ( 'NONE',  ( 15.01439307471096463, 1.118969480519667048, -226.7488225241675366 ) ) ;
#698 = CARTESIAN_POINT ( 'NONE',  ( -7.534279315020126155, -14.09704863723370494, -220.2840498463326355 ) ) ;
#699 = CARTESIAN_POINT ( 'NONE',  ( 25.17176037151762813, 18.95054595444721102, -221.3490360113488862 ) ) ;
#700 = CARTESIAN_POINT ( 'NONE',  ( 21.63401512838748175, 0.000000000000000000, -77.51594804401857175 ) ) ;
#701 = CARTESIAN_POINT ( 'NONE',  ( -27.72233273893307981, -16.15685914833838410, -223.8945077613443289 ) ) ;
#702 = CARTESIAN_POINT ( 'NONE',  ( 3.160467108836292116, 14.95099014189016629, -228.9242958482614370 ) ) ;
#703 = CARTESIAN_POINT ( 'NONE',  ( 29.89309326230132058, 6.052383583152112223, -228.3539431708548477 ) ) ;
#704 = EDGE_CURVE ( 'NONE', #20426, #16938, #13106, .T. ) ;
#705 = CARTESIAN_POINT ( 'NONE',  ( -12.01777041390050726, 10.97692933293401474, -227.6853890888168053 ) ) ;
#706 = CARTESIAN_POINT ( 'NONE',  ( -9.747505956077446854, 15.39125695327449783, -233.2799778227147840 ) ) ;
#707 = CARTESIAN_POINT ( 'NONE',  ( 21.19180206786061405, -1.472355559550188264, -231.3901500139509722 ) ) ;
#708 = CARTESIAN_POINT ( 'NONE',  ( -5.472810246302690196, -26.30400724048815420, -218.4657170016378416 ) ) ;
#709 = ORIENTED_EDGE ( 'NONE', *, *, #8052, .T. ) ;
#710 = CARTESIAN_POINT ( 'NONE',  ( 5.625090746907006611, -14.93184515622287201, -221.0486942310484721 ) ) ;
#711 = FACE_OUTER_BOUND ( 'NONE', #8838, .T. ) ;
#712 = CARTESIAN_POINT ( 'NONE',  ( 22.18132842682159733, 5.591149267797686839, -232.0584733989884114 ) ) ;
#713 = CARTESIAN_POINT ( 'NONE',  ( 26.16486877413895584, -0.2437668799822691745, -230.8325409000573814 ) ) ;
#714 = CARTESIAN_POINT ( 'NONE',  ( -19.88402822078561627, -6.951120502836210413, -232.7962440186676361 ) ) ;
#715 = CARTESIAN_POINT ( 'NONE',  ( 5.668262076144046979, -25.28042871382391965, -216.8182873783340483 ) ) ;
#716 = CARTESIAN_POINT ( 'NONE',  ( 6.173705828530630768, 14.85108299334794957, -222.6284669816953112 ) ) ;
#717 = CARTESIAN_POINT ( 'NONE',  ( 0.000000000000000000, 0.000000000000000000, -77.51594804401857175 ) ) ;
#718 = CARTESIAN_POINT ( 'NONE',  ( -12.45629340980802269, 5.675423426979704367, -220.8874502847910719 ) ) ;
#719 = CARTESIAN_POINT ( 'NONE',  ( -10.84997096467605182, 25.01800101807719301, -232.4518260228253155 ) ) ;
#720 = CARTESIAN_POINT ( 'NONE',  ( -2.532949683519015949, 17.18298404079579100, -229.0924323441805086 ) ) ;
#721 = CARTESIAN_POINT ( 'NONE',  ( 11.97659261343968851, -3.740017786417877854, -223.6042415182018033 ) ) ;
#722 = VERTEX_POINT ( 'NONE', #4541 ) ;
#723 = CARTESIAN_POINT ( 'NONE',  ( 14.63115627273841923, 9.024791562541032874, -232.5054678133655841 ) ) ;
#724 = CARTESIAN_POINT ( 'NONE',  ( -17.07311071032027172, 18.59516984069744794, -230.9440421721702137 ) ) ;
#725 = CARTESIAN_POINT ( 'NONE',  ( 18.50073117969547098, -1.889592114545683987, -232.6396648696776026 ) ) ;
#726 = CARTESIAN_POINT ( 'NONE',  ( -5.056986327342952947, -15.36481113542577503, -220.7955371552936583 ) ) ;
#727 = CARTESIAN_POINT ( 'NONE',  ( -22.63401512838757057, 0.000000000000000000, 77.51594804401857175 ) ) ;
#728 = ORIENTED_EDGE ( 'NONE', *, *, #22146, .F. ) ;
#729 = CARTESIAN_POINT ( 'NONE',  ( 17.68508104102419409, 23.41266195669770767, -227.5327139115408954 ) ) ;
#730 = CARTESIAN_POINT ( 'NONE',  ( 14.87638776485545122, -7.040696290218329878, -226.6726542491997805 ) ) ;
#731 = CARTESIAN_POINT ( 'NONE',  ( 25.50000000000000000, 0.5000000000000000000, 0.000000000000000000 ) ) ;
#732 = CARTESIAN_POINT ( 'NONE',  ( -1.643553855084622928, -13.05119293000219294, -222.7191902239112551 ) ) ;
#733 = PRODUCT_CONTEXT ( 'NONE', #18778, 'mechanical' ) ;
#734 = CARTESIAN_POINT ( 'NONE',  ( 5.169766346882679997, 29.28517558595074988, -221.5178724947562614 ) ) ;
#735 = CARTESIAN_POINT ( 'NONE',  ( -10.95054816480499760, 8.339404316518379545, -224.1596700080921778 ) ) ;
#736 = ORIENTED_EDGE ( 'NONE', *, *, #485, .T. ) ;
#737 = CARTESIAN_POINT ( 'NONE',  ( -12.31207293045244988, 6.732038552366256923, -221.0952066824360713 ) ) ;
#738 = CARTESIAN_POINT ( 'NONE',  ( -17.01799258133205228, -17.74971190556693657, -217.5843211863294755 ) ) ;
#739 = PLANE ( 'NONE',  #21317 ) ;
#740 = LINE ( 'NONE', #2534, #17773 ) ;
#741 = CARTESIAN_POINT ( 'NONE',  ( -3.060450601941519189, 13.29454208326677289, -222.0135664617158682 ) ) ;
#742 = CARTESIAN_POINT ( 'NONE',  ( 0.8130732720878883768, -26.02312037787507393, -216.7203152272084878 ) ) ;
#743 = CARTESIAN_POINT ( 'NONE',  ( 14.67391514392257612, -1.621881806925726588, -222.4758702327235653 ) ) ;
#744 = CARTESIAN_POINT ( 'NONE',  ( -9.443239614166923701, 9.388015667058336788, -222.3195230688234290 ) ) ;
#745 = CARTESIAN_POINT ( 'NONE',  ( -13.33011381921379090, 5.829915729572584304, -219.4453182727427816 ) ) ;
#746 = ADVANCED_FACE ( 'NONE', ( #18285 ), #1172, .T. ) ;
#747 = CARTESIAN_POINT ( 'NONE',  ( -2.125813515909480866, 15.68152656492264363, -220.3943115937447317 ) ) ;
#748 = DIRECTION ( 'NONE',  ( -0.000000000000000000, -1.000000000000000000, 0.000000000000000000 ) ) ;
#749 = CARTESIAN_POINT ( 'NONE',  ( 13.80707869872719762, 6.429545566348308760, -225.7152177910682553 ) ) ;
#750 = CARTESIAN_POINT ( 'NONE',  ( -9.995627826723184839, -14.18420632236771439, -221.4333122433492633 ) ) ;
#751 = ADVANCED_FACE ( 'NONE', ( #21864, #18061 ), #2957, .F. ) ;
#752 = CARTESIAN_POINT ( 'NONE',  ( 11.01659168199870287, 19.17922986229587323, -233.3715978632214387 ) ) ;
#753 = CARTESIAN_POINT ( 'NONE',  ( -11.82020046940938407, 10.16362659047642758, -224.3364193436540575 ) ) ;
#754 = CARTESIAN_POINT ( 'NONE',  ( -11.11821474075380678, 16.53100589793018926, -232.3736596382188395 ) ) ;
#755 = CARTESIAN_POINT ( 'NONE',  ( -27.94976817795961210, -4.610981384744690104, -229.1808304932418139 ) ) ;
#756 = EDGE_CURVE ( 'NONE', #14896, #1959, #16705, .T. ) ;
#757 = DIRECTION ( 'NONE',  ( 0.000000000000000000, 1.000000000000000000, -0.000000000000000000 ) ) ;
#758 = VERTEX_POINT ( 'NONE', #15024 ) ;
#759 = CARTESIAN_POINT ( 'NONE',  ( -20.54164754914381064, 7.122791156791981493, -233.5720402887671980 ) ) ;
#760 = CARTESIAN_POINT ( 'NONE',  ( 4.144298419883110540, -16.00443160190133085, -221.4341300285535965 ) ) ;
#761 = CARTESIAN_POINT ( 'NONE',  ( 0.000000000000000000, -23.00000000000000000, -24.99999999999999645 ) ) ;
#762 = CARTESIAN_POINT ( 'NONE',  ( 1.382955251742491898, 16.46353944795171032, -231.7743150979565030 ) ) ;
#763 = FACE_OUTER_BOUND ( 'NONE', #5768, .T. ) ;
#764 = CARTESIAN_POINT ( 'NONE',  ( 20.92846067405557520, -2.114533307883533109, -233.2756072794335580 ) ) ;
#765 = CARTESIAN_POINT ( 'NONE',  ( 15.33651282626308010, 7.807290788239344970, -218.6940806506825652 ) ) ;
#766 = CARTESIAN_POINT ( 'NONE',  ( 22.84140515590350518, 18.29101041979067332, -226.2334522600520472 ) ) ;
#767 = DIRECTION ( 'NONE',  ( -0.000000000000000000, -1.000000000000000000, -0.000000000000000000 ) ) ;
#768 = CARTESIAN_POINT ( 'NONE',  ( -9.606889355748592152, -11.26588727105406385, -229.9123324032181586 ) ) ;
#769 = CARTESIAN_POINT ( 'NONE',  ( 1.780803752597676537, -13.83832444325970101, -229.2250779460899537 ) ) ;
#770 = CARTESIAN_POINT ( 'NONE',  ( 26.00000000000000000, 1.371657349757716727E-13, 9.000000000000001776 ) ) ;
#771 = CARTESIAN_POINT ( 'NONE',  ( -3.130305314451475418, 18.08417128930788209, -217.9058652980469333 ) ) ;
#772 = CARTESIAN_POINT ( 'NONE',  ( 30.30544834784952002, -1.486206387887903047, -219.3838232483325896 ) ) ;
#773 = CARTESIAN_POINT ( 'NONE',  ( 22.14341918773124362, -7.622004812940091689, -217.4502831791021720 ) ) ;
#774 = CARTESIAN_POINT ( 'NONE',  ( -14.94640692938030746, 5.382918922058764544, -220.5478552936960455 ) ) ;
#775 = CARTESIAN_POINT ( 'NONE',  ( 11.63337745479824292, 8.229076005436313679, -220.5472098800687206 ) ) ;
#776 = CARTESIAN_POINT ( 'NONE',  ( 18.90025403853754327, 17.70150481658638952, -229.5234643039372315 ) ) ;
#777 = ORIENTED_EDGE ( 'NONE', *, *, #1994, .F. ) ;
#778 = CARTESIAN_POINT ( 'NONE',  ( 15.43677305580571435, -6.701975615562529853, -215.9934368197604897 ) ) ;
#779 = CARTESIAN_POINT ( 'NONE',  ( 0.4310340159982882779, 14.49716617963122189, 93.00000000000001421 ) ) ;
#780 = CIRCLE ( 'NONE', #11560, 22.91388766833460977 ) ;
#781 = CARTESIAN_POINT ( 'NONE',  ( 4.952019330116582907, 28.88045068338265509, -217.6369327391592208 ) ) ;
#782 = CARTESIAN_POINT ( 'NONE',  ( -5.467362224022371819, 23.92882567691090046, -234.7811165710531611 ) ) ;
#783 = CARTESIAN_POINT ( 'NONE',  ( -17.83852468596024110, -8.357198216422425219, -233.0481596892792879 ) ) ;
#784 = CARTESIAN_POINT ( 'NONE',  ( -9.749377714296398878, 10.28442384816749922, -229.3722863967025205 ) ) ;
#785 = CARTESIAN_POINT ( 'NONE',  ( 0.000000000000000000, 25.00000000000000000, -75.00000000000000000 ) ) ;
#786 = DIRECTION ( 'NONE',  ( -0.000000000000000000, 0.000000000000000000, -1.000000000000000000 ) ) ;
#787 = ADVANCED_FACE ( 'NONE', ( #3181 ), #2218, .F. ) ;
#788 = CIRCLE ( 'NONE', #14454, 19.63401512838747820 ) ;
#789 = CARTESIAN_POINT ( 'NONE',  ( -8.900302563431933933, 20.17395648083808268, -216.9116515890487733 ) ) ;
#790 = CARTESIAN_POINT ( 'NONE',  ( 25.09997929702755926, 1.294103573351435221, -217.0485712200477906 ) ) ;
#791 = CARTESIAN_POINT ( 'NONE',  ( -26.74045434827795020, 12.41518252455047744, -220.4617428697642652 ) ) ;
#792 = CARTESIAN_POINT ( 'NONE',  ( 15.87442104186276381, 8.674488492264579520, -230.9702037640878416 ) ) ;
#793 = CARTESIAN_POINT ( 'NONE',  ( 15.37450427861381286, -5.898921106289613847E-14, -228.0000000000000853 ) ) ;
#794 = ORIENTED_EDGE ( 'NONE', *, *, #11036, .F. ) ;
#795 = CARTESIAN_POINT ( 'NONE',  ( 3.522445101072706475, 23.08420003150784439, -231.7850044194335055 ) ) ;
#796 = CARTESIAN_POINT ( 'NONE',  ( -21.52428768452188734, -21.65989873160339840, -225.4304055049964006 ) ) ;
#797 = CARTESIAN_POINT ( 'NONE',  ( 13.49011766416699842, 7.659170998773840111, -228.1905628957712793 ) ) ;
#798 = CARTESIAN_POINT ( 'NONE',  ( -7.215839073791710412, -12.32959168003491968, -224.1142876912989834 ) ) ;
#799 = CARTESIAN_POINT ( 'NONE',  ( 18.92955364685790798, 2.856280672885327832, -224.0526243428037105 ) ) ;
#800 = AXIS2_PLACEMENT_3D ( 'NONE', #3925, #7323, #14193 ) ;
#801 = CARTESIAN_POINT ( 'NONE',  ( -12.62195384480319582, 9.244619650382723819, -228.6283004876635516 ) ) ;
#802 = CARTESIAN_POINT ( 'NONE',  ( 0.000000000000000000, -23.00000000000000000, -30.00000000000000000 ) ) ;
#803 = CARTESIAN_POINT ( 'NONE',  ( -29.01652113304903935, -3.607535226192160049, -222.1063433863846228 ) ) ;
#804 = CARTESIAN_POINT ( 'NONE',  ( 3.241594727517011609, 27.64703009302456138, -225.5540025036233374 ) ) ;
#805 = CARTESIAN_POINT ( 'NONE',  ( -10.29720673141181209, 11.14783905173092649, -222.8560683878917530 ) ) ;
#806 = CARTESIAN_POINT ( 'NONE',  ( -26.98548179121306845, 3.096138561569834913, -233.8324893795610251 ) ) ;
#807 = CARTESIAN_POINT ( 'NONE',  ( -9.206457440458645891, -21.52042488620018545, -217.0715276568171248 ) ) ;
#808 = CARTESIAN_POINT ( 'NONE',  ( 16.67941620816951698, 4.093285459228785506, -217.1675623234529269 ) ) ;
#809 = DIRECTION ( 'NONE',  ( 1.000000000000000000, 0.000000000000000000, 0.000000000000000000 ) ) ;
#810 = CARTESIAN_POINT ( 'NONE',  ( -10.76360437932642533, -14.08317586560949408, -234.4387784497120890 ) ) ;
#811 = CARTESIAN_POINT ( 'NONE',  ( -0.7041916573665241152, 14.60214745152014437, -226.3818583194645555 ) ) ;
#812 = AXIS2_PLACEMENT_3D ( 'NONE', #10619, #3959, #20954 ) ;
#813 = CARTESIAN_POINT ( 'NONE',  ( 17.91327661571172314, 1.545939370248587075, -216.9938266089438912 ) ) ;
#814 = VECTOR ( 'NONE', #17946, 1000.000000000000000 ) ;
#815 = CARTESIAN_POINT ( 'NONE',  ( -6.094651895680649467, 13.59752566126439177, -221.0608041154719103 ) ) ;
#816 = CARTESIAN_POINT ( 'NONE',  ( 9.253342549662157523, 15.33540844142859605, -216.2601104504267937 ) ) ;
#817 = ORIENTED_EDGE ( 'NONE', *, *, #5810, .F. ) ;
#818 = CARTESIAN_POINT ( 'NONE',  ( 2.435323595375026073, -28.08909517487921192, -228.1503986837488469 ) ) ;
#819 = CARTESIAN_POINT ( 'NONE',  ( -4.253447013113726527, -22.64852647464574531, -232.0531923962242615 ) ) ;
#820 = CARTESIAN_POINT ( 'NONE',  ( 28.51464931495100785, 5.422321182929326966, -223.8116416110474347 ) ) ;
#821 = CARTESIAN_POINT ( 'NONE',  ( 17.02763684969102798, -14.67205317233652195, -233.2001291093645818 ) ) ;
#822 = CARTESIAN_POINT ( 'NONE',  ( 29.52516483900593158, -0.1522717672070824924, -221.3034020690409704 ) ) ;
#823 = CARTESIAN_POINT ( 'NONE',  ( -14.13781561609191328, -15.90667165809925621, -233.6615929499251649 ) ) ;
#824 = CARTESIAN_POINT ( 'NONE',  ( 9.253909228257674258, 17.69332415812615977, -230.9900471521432621 ) ) ;
#825 = DIRECTION ( 'NONE',  ( 1.000000000000000000, 0.000000000000000000, 0.000000000000000000 ) ) ;
#826 = CARTESIAN_POINT ( 'NONE',  ( -20.76981451797363576, 10.27702766794165257, -234.3988437453480742 ) ) ;
#827 = CARTESIAN_POINT ( 'NONE',  ( 0.2389779871941385414, 16.64595486589868045, -218.1658233406367629 ) ) ;
#828 = CARTESIAN_POINT ( 'NONE',  ( -3.071946796551161984, 23.17078151772539485, -231.0066194318698933 ) ) ;
#829 = CARTESIAN_POINT ( 'NONE',  ( 26.86542643433637423, 1.561297562127881511, -231.3515426572852505 ) ) ;
#830 = ORIENTED_EDGE ( 'NONE', *, *, #2939, .T. ) ;
#831 = AXIS2_PLACEMENT_3D ( 'NONE', #5353, #20662, #13482 ) ;
#832 = CARTESIAN_POINT ( 'NONE',  ( 6.491278574642851851, 13.23281603069746382, -229.0355254242266767 ) ) ;
#833 = CARTESIAN_POINT ( 'NONE',  ( -16.48883219358909713, 20.84100960965193394, -219.4392138569792507 ) ) ;
#834 = CARTESIAN_POINT ( 'NONE',  ( 15.06072304412464291, 3.291435955319735651, -218.8606307204261725 ) ) ;
#835 = CARTESIAN_POINT ( 'NONE',  ( -6.507186921339367380, -21.94905981650347826, -217.8194053188079238 ) ) ;
#836 = DIRECTION ( 'NONE',  ( 0.000000000000000000, 0.000000000000000000, -1.000000000000000000 ) ) ;
#837 = ORIENTED_EDGE ( 'NONE', *, *, #13199, .T. ) ;
#838 = CARTESIAN_POINT ( 'NONE',  ( 5.343558017910363667, 26.29639771561252459, -218.1010331760174665 ) ) ;
#839 = CARTESIAN_POINT ( 'NONE',  ( 16.20395612672116314, -10.90071921976151081, -219.5016540749954856 ) ) ;
#840 = DIRECTION ( 'NONE',  ( 1.000000000000000000, 0.000000000000000000, 0.000000000000000000 ) ) ;
#841 = CARTESIAN_POINT ( 'NONE',  ( -3.300598509645395584, -18.18730530649546395, -233.4303386612170925 ) ) ;
#842 = CARTESIAN_POINT ( 'NONE',  ( 0.000000000000000000, 0.000000000000000000, 0.000000000000000000 ) ) ;
#843 = CARTESIAN_POINT ( 'NONE',  ( -2.698926868850080041, 12.89339462271858316, -226.7595176699009585 ) ) ;
#845 = CARTESIAN_POINT ( 'NONE',  ( -4.154119475380428916, 11.54776298361823095, -227.0876712548254943 ) ) ;
#844 = CIRCLE ( 'NONE', #13436, 21.00000000000008171 ) ;
#846 = VERTEX_POINT ( 'NONE', #22098 ) ;
#847 = CARTESIAN_POINT ( 'NONE',  ( -12.90983082593748676, 14.84936372681532823, -233.8009687022269532 ) ) ;
#848 = CARTESIAN_POINT ( 'NONE',  ( -23.63383474287343589, -9.908731599815467916, -232.6396219513094081 ) ) ;
#849 = AXIS2_PLACEMENT_3D ( 'NONE', #7181, #9308, #14163 ) ;
#850 = CARTESIAN_POINT ( 'NONE',  ( -24.24755750141337174, -6.112543499224761590, 7.941049042234675781 ) ) ;
#851 = CARTESIAN_POINT ( 'NONE',  ( 14.96415947227435339, -1.927366939720012606, -222.7010313878448358 ) ) ;
#852 = CARTESIAN_POINT ( 'NONE',  ( -18.70100282803782576, 16.58357028540773115, -216.4425743468854080 ) ) ;
#853 = CARTESIAN_POINT ( 'NONE',  ( -3.877698871368953082, -12.59008950621349676, -229.3284496285515388 ) ) ;
#854 = CARTESIAN_POINT ( 'NONE',  ( 28.22932473237819551, -8.039268142081398949, -226.6539694142420558 ) ) ;
#855 = CARTESIAN_POINT ( 'NONE',  ( -18.39892766464214446, 25.11039525536027739, -225.3444503920457294 ) ) ;
#856 = CARTESIAN_POINT ( 'NONE',  ( -28.99982533490676317, 5.894721259135065949, -231.5937499788843468 ) ) ;
#857 = CARTESIAN_POINT ( 'NONE',  ( -0.7292515499105728383, 28.18841485102515776, -220.8637599502617093 ) ) ;
#858 = CARTESIAN_POINT ( 'NONE',  ( 26.00000000000000000, -0.5000000000000000000, 0.000000000000000000 ) ) ;
#859 = CARTESIAN_POINT ( 'NONE',  ( 26.92457506054779515, 6.538608665672222209, -219.8654465082432807 ) ) ;
#860 = CARTESIAN_POINT ( 'NONE',  ( -8.182256202386261279, -21.48229377488409497, -218.8195705044138606 ) ) ;
#861 = EDGE_CURVE ( 'NONE', #21809, #17987, #12650, .T. ) ;
#862 = VERTEX_POINT ( 'NONE', #359 ) ;
#863 = CARTESIAN_POINT ( 'NONE',  ( 3.312424284731937618, 15.29837714273186045, -229.5209971419123747 ) ) ;
#864 = CARTESIAN_POINT ( 'NONE',  ( -15.95412330064426065, 13.09400588185824077, -218.6613039563597169 ) ) ;
#865 = CARTESIAN_POINT ( 'NONE',  ( -15.63515374589483109, 24.59141623553136569, -226.9057426066772507 ) ) ;
#866 = CARTESIAN_POINT ( 'NONE',  ( 21.96352831578812115, -0.3315607655626495731, -233.9427286327413356 ) ) ;
#867 = FACE_OUTER_BOUND ( 'NONE', #7455, .T. ) ;
#868 = ORIENTED_EDGE ( 'NONE', *, *, #19516, .F. ) ;
#869 = CARTESIAN_POINT ( 'NONE',  ( 19.29259174080182504, 0.5828707127177102931, -219.2781652733668807 ) ) ;
#870 = CARTESIAN_POINT ( 'NONE',  ( -5.974374721719333259, -11.49502099717533454, -225.7652523315031488 ) ) ;
#871 = CARTESIAN_POINT ( 'NONE',  ( 15.44226594370987726, 1.149341673865845959, -227.7740803137426724 ) ) ;
#872 = VECTOR ( 'NONE', #84, 1000.000000000000000 ) ;
#873 = CARTESIAN_POINT ( 'NONE',  ( -0.9414827276148034496, 23.96885519606619752, -216.4491898092606164 ) ) ;
#874 = CARTESIAN_POINT ( 'NONE',  ( 14.69910494674137702, -2.970304755374192585, -224.5345499258161794 ) ) ;
#875 = UNCERTAINTY_MEASURE_WITH_UNIT (LENGTH_MEASURE( 1.000000000000000082E-05 ), #1097, 'distance_accuracy_value', 'NONE');
#876 = ADVANCED_FACE ( 'NONE', ( #9133 ), #19112, .T. ) ;
#877 = CARTESIAN_POINT ( 'NONE',  ( 13.85822045549773129, -1.469587484828172919, -226.8778453516271156 ) ) ;
#878 = CARTESIAN_POINT ( 'NONE',  ( 9.818699534354031755, 13.69084898312510390, -233.4870046949650089 ) ) ;
#879 = CARTESIAN_POINT ( 'NONE',  ( 17.60676319847677007, 21.31475060840986302, -219.8266339603936785 ) ) ;
#880 = CARTESIAN_POINT ( 'NONE',  ( 0.000000000000000000, 0.000000000000000000, -60.00000000000001421 ) ) ;
#881 = CARTESIAN_POINT ( 'NONE',  ( -13.44328839870790837, -7.440897691988615392, -217.2299511873609106 ) ) ;
#882 = CARTESIAN_POINT ( 'NONE',  ( -15.22366728182010043, -5.552021002219007961, -230.2511309519622671 ) ) ;
#883 = CARTESIAN_POINT ( 'NONE',  ( 1.665334536937735568E-13, -23.00000000000006395, 75.00000000000000000 ) ) ;
#884 = CIRCLE ( 'NONE', #1615, 21.00000000000008527 ) ;
#885 = CARTESIAN_POINT ( 'NONE',  ( 0.000000000000000000, 0.000000000000000000, -55.00000000000000711 ) ) ;
#886 = CARTESIAN_POINT ( 'NONE',  ( -9.350291727197115321, 27.53754332352430367, -230.1504993026967441 ) ) ;
#887 = CARTESIAN_POINT ( 'NONE',  ( 26.46513128492211564, -16.79977778982552650, -229.3906297761492681 ) ) ;
#888 = CARTESIAN_POINT ( 'NONE',  ( 20.15756451863428111, -2.090604891399794774, -217.8900786001194945 ) ) ;
#889 = PRESENTATION_LAYER_ASSIGNMENT (  '', '', ( #21375 ) ) ;
#890 = CARTESIAN_POINT ( 'NONE',  ( -16.32047052250102581, 2.570795953410685009, -230.9329235942756213 ) ) ;
#891 = CARTESIAN_POINT ( 'NONE',  ( 18.81274554574540403, 10.85963742466947224, -234.0446454529665345 ) ) ;
#892 = CARTESIAN_POINT ( 'NONE',  ( 8.250760074138732136, 14.96691001493985951, -221.7548416114337613 ) ) ;
#893 = ORIENTED_EDGE ( 'NONE', *, *, #15181, .F. ) ;
#894 = CARTESIAN_POINT ( 'NONE',  ( 1.792482182455914064, -21.59191373485632681, -217.1959973011389593 ) ) ;
#895 = CARTESIAN_POINT ( 'NONE',  ( -4.825543794723682112, 13.95218839875094829, 93.00000000000001421 ) ) ;
#896 = CARTESIAN_POINT ( 'NONE',  ( -5.191169535941942748, 31.49570301054888688, -227.4714364261087098 ) ) ;
#897 = CARTESIAN_POINT ( 'NONE',  ( -4.877547524699579640, 12.94924496403020697, -219.3991240521417581 ) ) ;
#898 = CARTESIAN_POINT ( 'NONE',  ( 25.79934686323926840, -4.908228874239597417, -218.4849570602390543 ) ) ;
#899 = CARTESIAN_POINT ( 'NONE',  ( -11.26857159993117996, 28.96895336474501192, -225.6039696848669678 ) ) ;
#900 = CYLINDRICAL_SURFACE ( 'NONE', #10131, 17.50000000000000711 ) ;
#901 = CIRCLE ( 'NONE', #21740, 3.000000000000002665 ) ;
#902 = CARTESIAN_POINT ( 'NONE',  ( 2.770531592831002143, 22.28948935999365943, -215.1307751200139649 ) ) ;
#903 = CARTESIAN_POINT ( 'NONE',  ( 14.29548763234129538, 2.320071712424730315, -230.2610858871018422 ) ) ;
#904 = CARTESIAN_POINT ( 'NONE',  ( -27.29953305526601426, 11.21644211419729054, -229.3676346105362995 ) ) ;
#905 = CARTESIAN_POINT ( 'NONE',  ( 14.22574309452842733, 4.476723532073429546, -225.5862451792618231 ) ) ;
#906 = CARTESIAN_POINT ( 'NONE',  ( 15.61471550013173548, 0.4039561045782734117, -227.9741642728169211 ) ) ;
#907 = ORIENTED_EDGE ( 'NONE', *, *, #1716, .T. ) ;
#908 = CARTESIAN_POINT ( 'NONE',  ( -1.386728072030569692, 16.52832439466973824, -230.7516952943509807 ) ) ;
#909 = CARTESIAN_POINT ( 'NONE',  ( -22.23616899077527975, -11.51447210886970751, -217.5950109096934568 ) ) ;
#910 = CARTESIAN_POINT ( 'NONE',  ( 15.76910524310159900, 5.601482066865847820, -220.3440822020379528 ) ) ;
#911 = CARTESIAN_POINT ( 'NONE',  ( -3.600307272616782406, -16.89541809348436630, -217.5924753110707570 ) ) ;
#912 = CARTESIAN_POINT ( 'NONE',  ( 0.000000000000000000, 0.000000000000000000, 93.00000000000000000 ) ) ;
#913 = CARTESIAN_POINT ( 'NONE',  ( -25.19248792833826300, 13.40115236862232528, -221.2817950683888455 ) ) ;
#914 = DIRECTION ( 'NONE',  ( -1.000000000000000000, 0.000000000000000000, 0.000000000000000000 ) ) ;
#915 = CARTESIAN_POINT ( 'NONE',  ( 8.211296573249146746, -12.45047565346596130, -222.1279395315445413 ) ) ;
#916 = CARTESIAN_POINT ( 'NONE',  ( 13.41709597927210496, 19.57823531746157997, -218.2666972400567147 ) ) ;
#917 = CARTESIAN_POINT ( 'NONE',  ( -22.04240660558204823, 19.10355008918698871, -223.9524535985323723 ) ) ;
#918 = CARTESIAN_POINT ( 'NONE',  ( -10.98447002683091256, 8.146786682930290624, -230.8316952156193338 ) ) ;
#919 = CARTESIAN_POINT ( 'NONE',  ( -15.58915292315067802, -7.289217648355976742, -221.6802381019405175 ) ) ;
#920 = VECTOR ( 'NONE', #9719, 1000.000000000000000 ) ;
#921 = CARTESIAN_POINT ( 'NONE',  ( 29.33969601628096768, 11.98971187598327504, -225.2039690377576733 ) ) ;
#922 = CARTESIAN_POINT ( 'NONE',  ( -21.50000000000000711, 0.000000000000000000, -55.00000000000000711 ) ) ;
#923 = CARTESIAN_POINT ( 'NONE',  ( -13.46535974834342220, -4.471564630954283359, -230.9063312536467834 ) ) ;
#924 = CARTESIAN_POINT ( 'NONE',  ( -3.996294969088721505, 28.80481464818193515, -222.8623509149411746 ) ) ;
#925 = EDGE_CURVE ( 'NONE', #4211, #12391, #16929, .T. ) ;
#926 = CARTESIAN_POINT ( 'NONE',  ( 12.23284375931666013, 4.108221165122169616, -224.0993108960438462 ) ) ;
#927 = CARTESIAN_POINT ( 'NONE',  ( -6.496078068315311427, 23.46891392553531119, -233.1042179568201220 ) ) ;
#928 = CARTESIAN_POINT ( 'NONE',  ( 10.35958063030883025, 8.003303894222913328, -225.9303204057916048 ) ) ;
#929 = VECTOR ( 'NONE', #5748, 1000.000000000000000 ) ;
#930 = VERTEX_POINT ( 'NONE', #1922 ) ;
#931 = CARTESIAN_POINT ( 'NONE',  ( -0.6467335922136470128, -17.26771294536504442, -230.4732896975262122 ) ) ;
#932 = MECHANICAL_DESIGN_GEOMETRIC_PRESENTATION_REPRESENTATION (  '', ( #4162 ), #19607 ) ;
#933 = CARTESIAN_POINT ( 'NONE',  ( 7.092430827040528740, -27.48041265710635628, -228.4891580147104548 ) ) ;
#934 = CARTESIAN_POINT ( 'NONE',  ( 20.58703255433590940, 0.4816031003617209372, -231.9427175861361263 ) ) ;
#935 = CARTESIAN_POINT ( 'NONE',  ( 17.15627899979664051, -18.64955541608202694, -217.1729447097152388 ) ) ;
#936 = CARTESIAN_POINT ( 'NONE',  ( -26.98579662683621194, -8.531126968542736222, -229.5232528995939845 ) ) ;
#937 = CARTESIAN_POINT ( 'NONE',  ( -5.420780812268581883, -12.08122409751860360, -226.5143039284326392 ) ) ;
#938 = CARTESIAN_POINT ( 'NONE',  ( 3.060417506408009469, 27.46204888741655026, -226.6022202862033623 ) ) ;
#939 = PRODUCT_DEFINITION_FORMATION_WITH_SPECIFIED_SOURCE ( 'ANY', '', #16966, .NOT_KNOWN. ) ;
#940 = DIRECTION ( 'NONE',  ( 1.000000000000000000, 0.000000000000000000, 0.000000000000000000 ) ) ;
#941 = CARTESIAN_POINT ( 'NONE',  ( -22.10934047915441170, 0.9940043559354162506, -215.0000000000000000 ) ) ;
#942 = CARTESIAN_POINT ( 'NONE',  ( 4.343013938751969505, 13.02036404005131587, -224.7825435359082178 ) ) ;
#943 = CARTESIAN_POINT ( 'NONE',  ( 0.6289891638115701067, 16.47510600144228832, -227.0521699048171342 ) ) ;
#944 = CARTESIAN_POINT ( 'NONE',  ( 13.17462184258262070, -16.01403271225657932, -214.6792330615317610 ) ) ;
#945 = VERTEX_POINT ( 'NONE', #13560 ) ;
#946 = CARTESIAN_POINT ( 'NONE',  ( 11.96568375430165254, 8.504117401580989721, -219.8633768076029753 ) ) ;
#947 = CARTESIAN_POINT ( 'NONE',  ( -11.86888352782322897, 15.29489941890347282, -218.1379771575364259 ) ) ;
#948 = CARTESIAN_POINT ( 'NONE',  ( -16.23590288079963173, 0.2625226423351309513, -226.8300841971807813 ) ) ;
#949 = CARTESIAN_POINT ( 'NONE',  ( -1.544051355262263225, -15.46116467022245011, -222.0171457641791903 ) ) ;
#951 = CARTESIAN_POINT ( 'NONE',  ( -1.322875655532295136, 1.500000000000000000, -105.0000000000000142 ) ) ;
#950 = AXIS2_PLACEMENT_3D ( 'NONE', #2433, #2106, #17539 ) ;
#952 = CARTESIAN_POINT ( 'NONE',  ( 0.000000000000000000, 21.00000000000006395, -75.00000000000000000 ) ) ;
#953 = CARTESIAN_POINT ( 'NONE',  ( 11.87982377808925527, 10.85265283465803421, -229.5027252913499183 ) ) ;
#954 = CARTESIAN_POINT ( 'NONE',  ( 11.49416291172809856, -12.02598964588280595, -221.0946228713814889 ) ) ;
#955 = EDGE_CURVE ( 'NONE', #17437, #15809, #17323, .T. ) ;
#956 = CARTESIAN_POINT ( 'NONE',  ( -18.14952719657095415, 1.368063294522122275, -218.0005379682515922 ) ) ;
#957 = CARTESIAN_POINT ( 'NONE',  ( -1.608171596096409806, -16.77465153034988887, -217.4618546331240054 ) ) ;
#958 = CARTESIAN_POINT ( 'NONE',  ( 4.730976410881341465, 17.65764351829336931, -217.6025626048331674 ) ) ;
#959 = PRODUCT_DEFINITION_FORMATION_WITH_SPECIFIED_SOURCE ( 'ANY', '', #18761, .NOT_KNOWN. ) ;
#960 = CARTESIAN_POINT ( 'NONE',  ( 3.714886539878811789, 12.88803176524806560, -219.5889136906770034 ) ) ;
#961 = EDGE_LOOP ( 'NONE', ( #6548, #6973, #3988, #4970 ) ) ;
#962 = CARTESIAN_POINT ( 'NONE',  ( -17.39699619235753048, 15.64332637722790054, -216.0406373264262641 ) ) ;
#963 = CARTESIAN_POINT ( 'NONE',  ( -14.28784611495131784, -7.281039336628973402, -230.6208668958216208 ) ) ;
#964 = CARTESIAN_POINT ( 'NONE',  ( -24.94801726869080483, -1.644149540150739774, 9.869507958217397459 ) ) ;
#965 = CARTESIAN_POINT ( 'NONE',  ( -20.71238021041400756, 9.999865301160326680, 0.3337829719016462415 ) ) ;
#966 = CARTESIAN_POINT ( 'NONE',  ( -7.395406416482832590, 12.93623984139929739, -219.2606224730616873 ) ) ;
#967 = CARTESIAN_POINT ( 'NONE',  ( -3.564252528062037406, -12.01378896085460291, -227.6748268428467270 ) ) ;
#968 = CARTESIAN_POINT ( 'NONE',  ( 14.83290459615719215, -2.296615622475745688, -226.9301701175285757 ) ) ;
#969 = CARTESIAN_POINT ( 'NONE',  ( -15.66530208164916260, 23.23467148471576849, -218.1250122661128046 ) ) ;
#970 = CARTESIAN_POINT ( 'NONE',  ( -12.13127060986278316, 5.971392262169284315, -229.0615017441034524 ) ) ;
#971 = EDGE_LOOP ( 'NONE', ( #14065, #167, #6463, #2530 ) ) ;
#972 = CARTESIAN_POINT ( 'NONE',  ( 5.248013545904832711, 18.51731616863089158, -219.3673127389703552 ) ) ;
#973 = DIRECTION ( 'NONE',  ( -1.000000000000000000, 0.000000000000000000, 0.000000000000000000 ) ) ;
#974 = CARTESIAN_POINT ( 'NONE',  ( -12.12559971566433958, 1.856299769312002912, -227.8748781050665286 ) ) ;
#975 = CARTESIAN_POINT ( 'NONE',  ( -14.93084585968405875, -14.53813297593447373, -219.1962364975631772 ) ) ;
#976 = ORIENTED_EDGE ( 'NONE', *, *, #5207, .F. ) ;
#977 = CARTESIAN_POINT ( 'NONE',  ( 15.37089934297015503, 20.64239674606488961, -217.2018742121147170 ) ) ;
#978 = CARTESIAN_POINT ( 'NONE',  ( 2.276720224425493821, 13.44951395023989171, -229.9230017221896105 ) ) ;
#979 = CARTESIAN_POINT ( 'NONE',  ( 30.81364357021286793, -2.580535071768633060, -224.0234450364292513 ) ) ;
#980 = CARTESIAN_POINT ( 'NONE',  ( 0.000000000000000000, 0.000000000000000000, 95.00000000000000000 ) ) ;
#981 = ORIENTED_EDGE ( 'NONE', *, *, #19244, .F. ) ;
#982 = CARTESIAN_POINT ( 'NONE',  ( 18.69835413980967687, -1.262199651413310031, -230.6153330080101966 ) ) ;
#983 = EDGE_CURVE ( 'NONE', #1365, #10566, #7340, .T. ) ;
#984 = CARTESIAN_POINT ( 'NONE',  ( -3.496415903701482808, -16.44974864882642152, -218.6042005240371111 ) ) ;
#985 = CARTESIAN_POINT ( 'NONE',  ( 24.03642272140365677, 3.646960756862087205, -218.2320643939070806 ) ) ;
#986 = CARTESIAN_POINT ( 'NONE',  ( -10.24288955603410933, 28.30762631303078791, -220.8855665231519083 ) ) ;
#987 = DIRECTION ( 'NONE',  ( 0.000000000000000000, 0.000000000000000000, -1.000000000000000000 ) ) ;
#988 = CARTESIAN_POINT ( 'NONE',  ( 13.70635042947887428, -1.390919209824193592, -225.3477037409554953 ) ) ;
#989 = EDGE_CURVE ( 'NONE', #18158, #1422, #13733, .T. ) ;
#990 = CARTESIAN_POINT ( 'NONE',  ( 11.20580770355584299, 27.81589616365139150, -231.3138133330081132 ) ) ;
#991 = SHAPE_REPRESENTATION_RELATIONSHIP ( 'NONE' , 'NONE' ,  #6134, #7772 ) ;
#992 = DIRECTION ( 'NONE',  ( 1.000000000000000000, 0.000000000000000000, 0.000000000000000000 ) ) ;
#993 = CARTESIAN_POINT ( 'NONE',  ( 25.80927844399814930, 11.21489550116160316, -221.3538377621514996 ) ) ;
#994 = LINE ( 'NONE', #19555, #3715 ) ;
#995 = CARTESIAN_POINT ( 'NONE',  ( 14.68060984531904012, -6.704174034294832829, -225.1581031080203559 ) ) ;
#996 = CARTESIAN_POINT ( 'NONE',  ( -25.61235545225478560, -15.41032726095661509, -226.9890212492312855 ) ) ;
#997 = CARTESIAN_POINT ( 'NONE',  ( 0.000000000000000000, 0.000000000000000000, -78.50000000000000000 ) ) ;
#998 = CYLINDRICAL_SURFACE ( 'NONE', #19140, 23.00000000000008882 ) ;
#999 = CARTESIAN_POINT ( 'NONE',  ( -6.072587425033909803, 24.65158735603439055, -217.4249768037189767 ) ) ;
#1000 = CARTESIAN_POINT ( 'NONE',  ( 25.69865375807269459, -17.81673768310515626, -220.5381737609034474 ) ) ;
#1001 = CARTESIAN_POINT ( 'NONE',  ( 22.44368505003003378, -11.72633196808685163, -232.1179326287041533 ) ) ;
#1002 = CARTESIAN_POINT ( 'NONE',  ( -26.19327040236159831, 13.44417515682194875, -223.7810975255189874 ) ) ;
#1003 = CARTESIAN_POINT ( 'NONE',  ( 24.81079154715000357, 3.171651085595392772, -216.4177249688571578 ) ) ;
#1004 = CARTESIAN_POINT ( 'NONE',  ( 20.22510869507564024, 17.05975164568011238, -220.7829296213589316 ) ) ;
#1005 = ORIENTED_EDGE ( 'NONE', *, *, #4139, .T. ) ;
#1006 = CARTESIAN_POINT ( 'NONE',  ( 8.821624174887295666, -16.56651460208862758, -234.0193988870521196 ) ) ;
#1007 = CARTESIAN_POINT ( 'NONE',  ( 6.453512288987237611, 13.27786176931083695, 93.00000000000000000 ) ) ;
#1008 = CARTESIAN_POINT ( 'NONE',  ( -1.302381543002304687, 18.65968181418110206, -215.1730913991678449 ) ) ;
#1009 = CARTESIAN_POINT ( 'NONE',  ( 4.719925043692215993, 22.16918918211828782, -214.6883144083888908 ) ) ;
#1010 = CARTESIAN_POINT ( 'NONE',  ( 21.29805123434030634, -10.14609140759417905, -218.4136040999194108 ) ) ;
#1011 = CARTESIAN_POINT ( 'NONE',  ( -8.823862513872974489, 14.92351368520778898, -217.1499513473673346 ) ) ;
#1012 = CARTESIAN_POINT ( 'NONE',  ( 13.08434944240164022, -7.394545551606342748, 92.99999999999998579 ) ) ;
#1013 = CARTESIAN_POINT ( 'NONE',  ( -5.727886109716582297, 15.25217619989539486, -230.5419623196804650 ) ) ;
#1014 = CARTESIAN_POINT ( 'NONE',  ( 29.96674103997387206, 4.060923908484647349, -228.5323681967686298 ) ) ;
#1015 = CARTESIAN_POINT ( 'NONE',  ( -22.11084984981285118, 10.96048252433489623, -216.6117774006995376 ) ) ;
#1016 = CARTESIAN_POINT ( 'NONE',  ( 16.00819137755116373, 4.595691552992191120, -229.5669508871464757 ) ) ;
#1017 = CARTESIAN_POINT ( 'NONE',  ( 9.489894741926459432, 25.96007012349547338, -222.3210984495278524 ) ) ;
#1018 = CARTESIAN_POINT ( 'NONE',  ( 15.50065424546137827, 0.1434261877680026442, -227.9977536057407690 ) ) ;
#1019 = ORIENTED_EDGE ( 'NONE', *, *, #7643, .T. ) ;
#1020 = CARTESIAN_POINT ( 'NONE',  ( 6.685304925496912354, 17.61973327427626046, -230.4152170797364931 ) ) ;
#1021 = CARTESIAN_POINT ( 'NONE',  ( -11.39823187951283501, -7.998194509987097689, -226.8062974464413912 ) ) ;
#1022 = CARTESIAN_POINT ( 'NONE',  ( 15.89706143421296147, 10.57416387607782227, -218.3862415393350318 ) ) ;
#1023 = CARTESIAN_POINT ( 'NONE',  ( -7.879270980303660465, -15.58863178937888350, -218.8267223810934752 ) ) ;
#1024 = DIRECTION ( 'NONE',  ( 1.000000000000000000, 0.000000000000000000, 0.000000000000000000 ) ) ;
#1025 = CARTESIAN_POINT ( 'NONE',  ( -26.11114532382342901, 12.73400870066318902, -227.7653936945517046 ) ) ;
#1026 = CARTESIAN_POINT ( 'NONE',  ( 19.33791609681259160, -22.44220124466257360, -223.0821732511882090 ) ) ;
#1027 = EDGE_CURVE ( 'NONE', #7787, #237, #6904, .T. ) ;
#1028 = CARTESIAN_POINT ( 'NONE',  ( 10.97349919442152810, 9.416813005082010690, -227.3764328406868742 ) ) ;
#1029 = CARTESIAN_POINT ( 'NONE',  ( -12.43544732248594720, 12.69828336922617318, -219.3367909706387877 ) ) ;
#1031 = AXIS2_PLACEMENT_3D ( 'NONE', #727, #2413, #7826 ) ;
#1030 = CARTESIAN_POINT ( 'NONE',  ( -12.61443312487471324, 8.399394471292156439, -217.5740162615319093 ) ) ;
#1032 = CARTESIAN_POINT ( 'NONE',  ( -24.13290183362846264, -6.995619630784887022, -220.0347092962472288 ) ) ;
#1033 = ADVANCED_FACE ( 'NONE', ( #15252 ), #17682, .F. ) ;
#1034 = CARTESIAN_POINT ( 'NONE',  ( 11.17228388010293649, 5.622653638471959425, -222.3672781564363845 ) ) ;
#1035 = FACE_OUTER_BOUND ( 'NONE', #14806, .T. ) ;
#1036 = CARTESIAN_POINT ( 'NONE',  ( -15.94006964721192432, -5.209069452486915885, -233.2212940081757040 ) ) ;
#1037 = CARTESIAN_POINT ( 'NONE',  ( 8.175342817246784577, 19.41817470142738244, -216.6818271833384699 ) ) ;
#1038 = CARTESIAN_POINT ( 'NONE',  ( -21.48978835671764287, 1.062155088816892468, -219.0000000007146355 ) ) ;
#1039 = CARTESIAN_POINT ( 'NONE',  ( -10.45265333418718612, 16.71118685480038479, -231.7490466715443631 ) ) ;
#1040 = CARTESIAN_POINT ( 'NONE',  ( 4.024086222410633518, 12.48004227094270746, -230.0177668608922374 ) ) ;
#1041 = ORIENTED_EDGE ( 'NONE', *, *, #7973, .T. ) ;
#1042 = CARTESIAN_POINT ( 'NONE',  ( 0.6118723529980315545, -20.11903950562274446, -217.9558718073025716 ) ) ;
#1043 = ORIENTED_EDGE ( 'NONE', *, *, #10914, .T. ) ;
#1044 = CARTESIAN_POINT ( 'NONE',  ( -6.723652888800149441, -28.28510889945508211, -226.1741921951756638 ) ) ;
#1045 = CARTESIAN_POINT ( 'NONE',  ( 16.38151749656409351, 8.902090001712490874, -231.2955017965201989 ) ) ;
#1046 = CARTESIAN_POINT ( 'NONE',  ( 13.82188917133564132, -5.740199443570373816, -227.9076376976435654 ) ) ;
#1047 = CARTESIAN_POINT ( 'NONE',  ( 30.21546680466445167, 0.1681144524405517038, -223.7059097242262737 ) ) ;
#1048 = CARTESIAN_POINT ( 'NONE',  ( -8.878187501988019648, -11.23476449186280846, -221.0271673637577123 ) ) ;
#1049 = CARTESIAN_POINT ( 'NONE',  ( 3.755404788550845474, 24.96758616565139022, -220.0839658302907935 ) ) ;
#1050 = CARTESIAN_POINT ( 'NONE',  ( 1.526556658859591000E-13, -22.63401512838754570, -77.51594804401857175 ) ) ;
#1051 = CARTESIAN_POINT ( 'NONE',  ( -16.40095417437164471, 2.582410108382750646, -233.5151473761628154 ) ) ;
#1052 = CARTESIAN_POINT ( 'NONE',  ( -0.9414827276148034496, 23.96885519606619752, -216.4491898092606164 ) ) ;
#1053 = CARTESIAN_POINT ( 'NONE',  ( 2.445562843591592372, 25.89340784564244657, -229.2671352353737859 ) ) ;
#1054 = CARTESIAN_POINT ( 'NONE',  ( 15.44393261315032184, -28.37553556939610999, -226.2064134899511600 ) ) ;
#1055 = CARTESIAN_POINT ( 'NONE',  ( 28.03290210476798094, 13.48017620089690638, -224.9212082181537937 ) ) ;
#1056 = CARTESIAN_POINT ( 'NONE',  ( -11.83954511762131112, 10.58068896997146346, -226.6171226499791089 ) ) ;
#1057 = CARTESIAN_POINT ( 'NONE',  ( -20.67624351032310059, -0.8683020119106035217, -219.0957770725675005 ) ) ;
#1058 = CARTESIAN_POINT ( 'NONE',  ( -6.749503758482277682, -23.22604375411988187, -218.1095993038993299 ) ) ;
#1059 = DIRECTION ( 'NONE',  ( -1.000000000000000000, 0.000000000000000000, 0.000000000000000000 ) ) ;
#1060 = DIRECTION ( 'NONE',  ( -0.000000000000000000, -0.000000000000000000, 1.000000000000000000 ) ) ;
#1061 = CARTESIAN_POINT ( 'NONE',  ( 15.85665641241444668, 18.24713744004561988, -217.7195292979064902 ) ) ;
#1062 = CARTESIAN_POINT ( 'NONE',  ( 13.74877878529187747, -9.499568690286848138, -221.9332727739125346 ) ) ;
#1063 = CARTESIAN_POINT ( 'NONE',  ( -24.15814485343234352, 4.373587128574028426, -232.6698675874553430 ) ) ;
#1064 = CARTESIAN_POINT ( 'NONE',  ( -9.078153229956912540, -10.71731945587431056, -228.5228069477245469 ) ) ;
#1065 = DIRECTION ( 'NONE',  ( 0.000000000000000000, 0.000000000000000000, 1.000000000000000000 ) ) ;
#1066 = CARTESIAN_POINT ( 'NONE',  ( 4.907833106823921376, 13.98151846258800290, -229.0190609869640923 ) ) ;
#1067 = CARTESIAN_POINT ( 'NONE',  ( 3.490829917597003895, 11.40812925993816229, -222.8973702487053004 ) ) ;
#1068 = ORIENTED_EDGE ( 'NONE', *, *, #14661, .F. ) ;
#1069 = CARTESIAN_POINT ( 'NONE',  ( -3.205260335674071648, 17.52234722004434531, -232.9754319808710363 ) ) ;
#1070 = CARTESIAN_POINT ( 'NONE',  ( -30.29980174031923923, -2.072322947205907706, -221.9291348703773679 ) ) ;
#1071 = CARTESIAN_POINT ( 'NONE',  ( -23.33371624899309893, -8.978322754191188082, -4.451123584478842155 ) ) ;
#1072 = DIRECTION ( 'NONE',  ( -2.891205793294678696E-17, 0.000000000000000000, -1.000000000000000000 ) ) ;
#1073 = CARTESIAN_POINT ( 'NONE',  ( -14.83974801774860630, 13.71714848582103485, -216.0935642439352762 ) ) ;
#1074 = CARTESIAN_POINT ( 'NONE',  ( -2.809719670556939608, -23.45209095268191390, -234.3886352793013543 ) ) ;
#1075 = CARTESIAN_POINT ( 'NONE',  ( 24.99999999999999645, 1.360023205165816762E-13, 10.00000000000000000 ) ) ;
#1076 = CARTESIAN_POINT ( 'NONE',  ( -15.58461825850822180, 18.91734573546571951, -233.7691177939990723 ) ) ;
#1077 = CARTESIAN_POINT ( 'NONE',  ( -12.79639481117843935, 1.974037863663017589, -229.6094308443170746 ) ) ;
#1078 = CARTESIAN_POINT ( 'NONE',  ( -0.4548635697939061306, 27.30478022265488036, -219.8474162243132071 ) ) ;
#1079 = DIRECTION ( 'NONE',  ( -0.000000000000000000, -0.000000000000000000, -1.000000000000000000 ) ) ;
#1080 = CARTESIAN_POINT ( 'NONE',  ( 22.37742875470728876, 11.29804624588327577, -218.9256858961603882 ) ) ;
#1081 = CARTESIAN_POINT ( 'NONE',  ( -6.877419757825867563, -14.31154863906730412, -224.3431884172090918 ) ) ;
#1082 = ORIENTED_EDGE ( 'NONE', *, *, #11545, .T. ) ;
#1083 = CARTESIAN_POINT ( 'NONE',  ( -15.11329978779464689, 11.41628732213579411, -231.7124318929555500 ) ) ;
#1084 = CARTESIAN_POINT ( 'NONE',  ( 10.95881707662767290, 12.06788758096456782, -231.4359029166177208 ) ) ;
#1085 = CARTESIAN_POINT ( 'NONE',  ( -4.021035526861677312, 25.02763064454595110, -216.6167103172201678 ) ) ;
#1086 = CARTESIAN_POINT ( 'NONE',  ( 14.79879825009101069, -3.130997509566451953, -219.4569190381675696 ) ) ;
#1087 = DIRECTION ( 'NONE',  ( -1.000000000000000000, 0.000000000000000000, 2.891205793294678696E-17 ) ) ;
#1088 = ORIENTED_EDGE ( 'NONE', *, *, #2868, .F. ) ;
#1089 = CARTESIAN_POINT ( 'NONE',  ( -13.58874046263339608, 12.73011668665171392, -216.5659449791897941 ) ) ;
#1090 = CARTESIAN_POINT ( 'NONE',  ( -15.77287877451090203, -21.23371664991514152, -233.2776952697515185 ) ) ;
#1091 = DIRECTION ( 'NONE',  ( -1.000000000000000000, 0.000000000000000000, 0.000000000000000000 ) ) ;
#1092 = CARTESIAN_POINT ( 'NONE',  ( 10.02513374692848913, 18.81568788741115128, -217.1505009242214612 ) ) ;
#1093 = PLANE ( 'NONE',  #20973 ) ;
#1094 = UNCERTAINTY_MEASURE_WITH_UNIT (LENGTH_MEASURE( 1.000000000000000082E-05 ), #8420, 'distance_accuracy_value', 'NONE');
#1095 = CARTESIAN_POINT ( 'NONE',  ( -15.10945752141584464, 6.470132813599071220, -220.1568141593501764 ) ) ;
#1096 = CARTESIAN_POINT ( 'NONE',  ( 13.09827881591457022, 28.40264942367575784, -221.1045935444571455 ) ) ;
#1097 =( LENGTH_UNIT ( ) NAMED_UNIT ( * ) SI_UNIT ( .MILLI., .METRE. ) );
#1098 = CARTESIAN_POINT ( 'NONE',  ( -24.94744066671306015, 1.651985823032437350, -9.868045913509542189 ) ) ;
#1099 = CARTESIAN_POINT ( 'NONE',  ( 16.54345861550681107, 19.37554510112122230, -218.2240151908141002 ) ) ;
#1100 = DIRECTION ( 'NONE',  ( -0.000000000000000000, -0.000000000000000000, 1.000000000000000000 ) ) ;
#1101 = CARTESIAN_POINT ( 'NONE',  ( 17.78543650172321833, -3.538499054913423869, -220.4382406111031401 ) ) ;
#1102 = AXIS2_PLACEMENT_3D ( 'NONE', #16266, #2525, #11420 ) ;
#1103 = CARTESIAN_POINT ( 'NONE',  ( -12.13177435108894642, -8.392035797555511323, -228.8392847287196332 ) ) ;
#1104 = CARTESIAN_POINT ( 'NONE',  ( -22.17508266256912819, -6.110112796411599767, -7.922854749118508622 ) ) ;
#1105 = DIRECTION ( 'NONE',  ( -0.000000000000000000, -0.000000000000000000, 1.000000000000000000 ) ) ;
#1106 = CARTESIAN_POINT ( 'NONE',  ( -1.238249567024760189, 29.30580384236933966, -223.2399636023643836 ) ) ;
#1107 = CARTESIAN_POINT ( 'NONE',  ( 15.19497947618244460, -8.176986896541109218, -234.2449823452919304 ) ) ;
#1108 = CARTESIAN_POINT ( 'NONE',  ( 22.14671607713456325, -14.13547298543019437, -218.1897693226341914 ) ) ;
#1109 = CARTESIAN_POINT ( 'NONE',  ( -13.97943781666340790, 5.798109546139844639, -228.2992319913466019 ) ) ;
#1110 = CARTESIAN_POINT ( 'NONE',  ( 14.33191776452776622, 5.147404080619256916, -219.0172570056664938 ) ) ;
#1111 = CARTESIAN_POINT ( 'NONE',  ( 12.94599882983645145, 15.82237817288049442, -219.3332542656393116 ) ) ;
#1112 = ORIENTED_EDGE ( 'NONE', *, *, #19320, .F. ) ;
#1113 = CARTESIAN_POINT ( 'NONE',  ( -0.09985864093865706725, -15.05342968659714309, -222.4585048042796132 ) ) ;
#1114 = FACE_OUTER_BOUND ( 'NONE', #21076, .T. ) ;
#1115 = CARTESIAN_POINT ( 'NONE',  ( -15.35982698007958724, 5.508237851081846159, -233.6994028941782631 ) ) ;
#1116 = CARTESIAN_POINT ( 'NONE',  ( 7.393167209263542539, 10.77319710117329699, -221.1179833906701049 ) ) ;
#1117 = CARTESIAN_POINT ( 'NONE',  ( -2.577721557973523314, 25.83760098923793791, -215.4660676095525389 ) ) ;
#1118 = CARTESIAN_POINT ( 'NONE',  ( 29.05460218321669785, -4.534277981440765437, -222.0637325791020373 ) ) ;
#1119 = CARTESIAN_POINT ( 'NONE',  ( -8.172572110426221670, 16.86653848210977813, -233.4220330256369493 ) ) ;
#1120 = CARTESIAN_POINT ( 'NONE',  ( -20.94800339253696109, 4.477632454355491731, -216.5423208360950298 ) ) ;
#1121 = CARTESIAN_POINT ( 'NONE',  ( 2.165130313308041288, 31.55305250914585002, -225.6791154433767304 ) ) ;
#1122 = CARTESIAN_POINT ( 'NONE',  ( -18.04102731735134313, 0.8647102676311391178, -229.4625228093430849 ) ) ;
#1123 = CARTESIAN_POINT ( 'NONE',  ( -15.15434969228324924, 4.423874646950748613, -230.6144467931089821 ) ) ;
#1124 = CARTESIAN_POINT ( 'NONE',  ( 18.76922974182421555, 13.12635134380198210, -217.8010375391909008 ) ) ;
#1125 = CARTESIAN_POINT ( 'NONE',  ( 2.445562843591592372, 25.89340784564244657, -229.2671352353737859 ) ) ;
#1126 = CARTESIAN_POINT ( 'NONE',  ( 1.665334536937734811E-13, -24.63401512838747820, 77.51594804401857175 ) ) ;
#1127 = DIRECTION ( 'NONE',  ( -1.000000000000000000, 0.000000000000000000, 0.000000000000000000 ) ) ;
#1128 = CARTESIAN_POINT ( 'NONE',  ( 8.539351012053531420, 16.03230746435535181, -220.6282946404833751 ) ) ;
#1129 = CARTESIAN_POINT ( 'NONE',  ( -14.76273180397945772, -6.370707202906876532, -220.0066229284273334 ) ) ;
#1130 = CARTESIAN_POINT ( 'NONE',  ( 17.00168025137501004, 6.212099629982537508, -219.0548246536471595 ) ) ;
#1131 = CARTESIAN_POINT ( 'NONE',  ( -5.234434610370643171, -17.78654814248861626, -233.1081320952062867 ) ) ;
#1132 = DIRECTION ( 'NONE',  ( 1.000000000000000000, 0.000000000000000000, 0.000000000000000000 ) ) ;
#1133 = AXIS2_PLACEMENT_3D ( 'NONE', #4423, #19514, #4101 ) ;
#1134 = CARTESIAN_POINT ( 'NONE',  ( -16.12870690754239078, 23.19263481078822053, -221.6099859194323471 ) ) ;
#1135 = SHAPE_REPRESENTATION_RELATIONSHIP ( 'NONE' , 'NONE' ,  #14642, #20620 ) ;
#1136 = CARTESIAN_POINT ( 'NONE',  ( 13.93061470302797389, -11.80544459979379646, -217.9389246709861538 ) ) ;
#1137 = CARTESIAN_POINT ( 'NONE',  ( 26.72610819325501907, 14.97064052581051108, -224.6384473985499426 ) ) ;
#1138 = CARTESIAN_POINT ( 'NONE',  ( -11.03778527004271659, 26.96286968643956428, -225.4057095641571209 ) ) ;
#1139 = CARTESIAN_POINT ( 'NONE',  ( -12.14471622011552832, 3.716031503296523653, -220.6237729066402835 ) ) ;
#1140 = CARTESIAN_POINT ( 'NONE',  ( -23.54933555373352050, -14.29320362656835997, -227.5895276738501423 ) ) ;
#1141 = EDGE_CURVE ( 'NONE', #12646, #6063, #20818, .T. ) ;
#1142 = CARTESIAN_POINT ( 'NONE',  ( 15.87399429023076003, -1.683916961781461552, -230.8621029165058758 ) ) ;
#1143 = AXIS2_PLACEMENT_3D ( 'NONE', #18620, #15780, #13440 ) ;
#1144 = CARTESIAN_POINT ( 'NONE',  ( 1.665334536937734811E-13, -23.00000000000000000, 69.99999999999998579 ) ) ;
#1145 = CARTESIAN_POINT ( 'NONE',  ( -18.48589171870721870, -21.38265182533571362, -233.2911668074952729 ) ) ;
#1146 = CARTESIAN_POINT ( 'NONE',  ( 20.26651059498356844, 18.95255124124090074, -231.7206897233655525 ) ) ;
#1147 = CARTESIAN_POINT ( 'NONE',  ( 25.50289296650958448, 5.998088869914441901, -233.1161630295026157 ) ) ;
#1148 = AXIS2_PLACEMENT_3D ( 'NONE', #12886, #17854, #11310 ) ;
#1149 = CARTESIAN_POINT ( 'NONE',  ( -4.021035526861677312, 25.02763064454595110, -216.6167103172201678 ) ) ;
#1150 = EDGE_CURVE ( 'NONE', #18699, #10116, #5395, .T. ) ;
#1151 = CARTESIAN_POINT ( 'NONE',  ( 12.46318849118074112, 25.01309605388695445, -216.9820503660967859 ) ) ;
#1152 = VERTEX_POINT ( 'NONE', #20394 ) ;
#1153 = CARTESIAN_POINT ( 'NONE',  ( 0.5598654370342924791, -17.79304497667748564, -219.0037976856824571 ) ) ;
#1154 = CARTESIAN_POINT ( 'NONE',  ( -6.507186921339367380, -21.94905981650347826, -217.8194053188079238 ) ) ;
#1155 = AXIS2_PLACEMENT_3D ( 'NONE', #10454, #3681, #5262 ) ;
#1156 = CARTESIAN_POINT ( 'NONE',  ( -13.91932826323387395, 8.983986115891950064, -216.4624824187541776 ) ) ;
#1157 = CARTESIAN_POINT ( 'NONE',  ( 17.28140336138120858, -11.48510652344925020, -216.9852223368602893 ) ) ;
#1158 = CARTESIAN_POINT ( 'NONE',  ( -18.34948365288241590, -1.907751280579004893, -231.5848060246952116 ) ) ;
#1159 = CARTESIAN_POINT ( 'NONE',  ( -21.28605893225895684, -20.43870967537180050, -221.0356759888913700 ) ) ;
#1160 = CARTESIAN_POINT ( 'NONE',  ( 16.73391517716289911, 11.95167056011791828, -233.0268722588312755 ) ) ;
#1161 = DIRECTION ( 'NONE',  ( 0.000000000000000000, 0.000000000000000000, 1.000000000000000000 ) ) ;
#1162 = CARTESIAN_POINT ( 'NONE',  ( -9.982417347796181062, 8.907629238417765549, -225.5124013436514474 ) ) ;
#1163 = CARTESIAN_POINT ( 'NONE',  ( 13.25330606581809789, 10.40242132629824034, -230.9170765704288044 ) ) ;
#1164 = CARTESIAN_POINT ( 'NONE',  ( 11.67669251569587985, 24.04736029062789981, -218.5856804285192254 ) ) ;
#1165 = CARTESIAN_POINT ( 'NONE',  ( 20.85755584069816493, 20.53615333921957742, -227.2010381488614996 ) ) ;
#1166 = CARTESIAN_POINT ( 'NONE',  ( 12.01003603113874441, -9.270215614621081457, -232.3219482526175170 ) ) ;
#1167 = CARTESIAN_POINT ( 'NONE',  ( 20.26651059498356844, 18.95255124124090074, -231.7206897233655525 ) ) ;
#1168 = CARTESIAN_POINT ( 'NONE',  ( -12.14452111807825041, 26.21581784948545035, -221.1455569020914140 ) ) ;
#1169 = CARTESIAN_POINT ( 'NONE',  ( -2.609511328024065602, -16.97143768612226822, -230.2205646068415490 ) ) ;
#1170 = CARTESIAN_POINT ( 'NONE',  ( -14.87984907657228639, 0.2138881189739126887, -228.7773920408832282 ) ) ;
#1171 = AXIS2_PLACEMENT_3D ( 'NONE', #5653, #12637, #8934 ) ;
#1172 = PLANE ( 'NONE',  #9056 ) ;
#1173 = AXIS2_PLACEMENT_3D ( 'NONE', #1126, #16330, #2912 ) ;
#1174 = CARTESIAN_POINT ( 'NONE',  ( 25.80927844399814930, 11.21489550116160316, -221.3538377621514996 ) ) ;
#1175 = CARTESIAN_POINT ( 'NONE',  ( 10.87273020620571629, -12.78363999705779186, -228.8712466752294858 ) ) ;
#1176 = PLANE ( 'NONE',  #1102 ) ;
#1177 = CARTESIAN_POINT ( 'NONE',  ( -10.11868820210310282, -13.51996935893276053, -218.1704188629865371 ) ) ;
#1178 = CARTESIAN_POINT ( 'NONE',  ( -0.9414827276148034496, 23.96885519606619752, -216.4491898092606164 ) ) ;
#1179 = CARTESIAN_POINT ( 'NONE',  ( 7.587775680576782200, 20.81864918083767435, -235.2547171215352364 ) ) ;
#1180 = ORIENTED_EDGE ( 'NONE', *, *, #8054, .T. ) ;
#1181 = CARTESIAN_POINT ( 'NONE',  ( -2.698926868850080041, 12.89339462271858316, -226.7595176699009585 ) ) ;
#1182 = CARTESIAN_POINT ( 'NONE',  ( 28.84595539031434797, -3.450543886267656735, -229.1532420603894877 ) ) ;
#1183 = CARTESIAN_POINT ( 'NONE',  ( 29.37495210618232022, -3.074218464324032229, -220.1817713028459025 ) ) ;
#1184 = CARTESIAN_POINT ( 'NONE',  ( 1.526556658859590243E-13, -21.80000000000000071, 78.50000000000000000 ) ) ;
#1185 = CARTESIAN_POINT ( 'NONE',  ( -3.082945806077231676, 30.69897765966285874, -224.2387254578930822 ) ) ;
#1186 = CARTESIAN_POINT ( 'NONE',  ( -13.54879968420069503, -27.67624318860520916, -230.2549257473255579 ) ) ;
#1187 = CARTESIAN_POINT ( 'NONE',  ( 13.47054497134856277, -24.75371201277411615, -218.7687119198782000 ) ) ;
#1188 = AXIS2_PLACEMENT_3D ( 'NONE', #7802, #21501, #4395 ) ;
#1189 = CARTESIAN_POINT ( 'NONE',  ( 20.98776729843937972, -13.55153944770713359, -217.5092423276211946 ) ) ;
#1190 = VECTOR ( 'NONE', #12712, 1000.000000000000000 ) ;
#1191 = CARTESIAN_POINT ( 'NONE',  ( 16.55609572527610851, 2.729108819536508967, -230.5704679660131831 ) ) ;
#1192 = CARTESIAN_POINT ( 'NONE',  ( 6.332229114051408203, 16.75791367489523154, -229.7702805136205200 ) ) ;
#1193 = CARTESIAN_POINT ( 'NONE',  ( -3.400000000000003908, 0.000000000000000000, -224.9999999999999716 ) ) ;
#1194 = CARTESIAN_POINT ( 'NONE',  ( -25.59521542166570640, 7.637420400166985424, -216.4190921938142935 ) ) ;
#1195 = CARTESIAN_POINT ( 'NONE',  ( -23.09090074015852778, -15.52172445179926896, -222.9863534629544972 ) ) ;
#1196 = EDGE_LOOP ( 'NONE', ( #14058, #1375, #16150, #10148 ) ) ;
#1197 = CARTESIAN_POINT ( 'NONE',  ( -12.82737030338386219, 8.595865151885988098, -221.6735325378515142 ) ) ;
#1198 = CARTESIAN_POINT ( 'NONE',  ( 2.535512286608554433, 13.86868953312499109, -224.9313928733152181 ) ) ;
#1199 = CARTESIAN_POINT ( 'NONE',  ( 2.291262277241625345, 17.20278591336981222, -216.2185160402476924 ) ) ;
#1200 = CARTESIAN_POINT ( 'NONE',  ( -22.73111095712577168, -10.24355154293710690, -230.8570942615963872 ) ) ;
#1201 = DIRECTION ( 'NONE',  ( 0.000000000000000000, 0.000000000000000000, -1.000000000000000000 ) ) ;
#1202 = ORIENTED_EDGE ( 'NONE', *, *, #20807, .F. ) ;
#1203 = CARTESIAN_POINT ( 'NONE',  ( -22.04257564474043818, 18.72061943465525857, -219.1781831295219263 ) ) ;
#1204 = CARTESIAN_POINT ( 'NONE',  ( -17.08385316318651448, -18.56764924811779949, -215.7277288032969977 ) ) ;
#1205 = CARTESIAN_POINT ( 'NONE',  ( 0.000000000000000000, 0.000000000000000000, 75.00000000000000000 ) ) ;
#1206 = CARTESIAN_POINT ( 'NONE',  ( 17.60676319847677007, 21.31475060840986302, -219.8266339603936785 ) ) ;
#1207 = DIRECTION ( 'NONE',  ( -1.000000000000000000, 0.000000000000000000, 0.000000000000000000 ) ) ;
#1208 = CIRCLE ( 'NONE', #18833, 3.000000000000002665 ) ;
#1209 = CONICAL_SURFACE ( 'NONE', #1910, 23.03038449397558196, 0.1745329251994333364 ) ;
#1210 = DIRECTION ( 'NONE',  ( 0.000000000000000000, 0.000000000000000000, 1.000000000000000000 ) ) ;
#1211 = EDGE_CURVE ( 'NONE', #9851, #16873, #2253, .T. ) ;
#1212 = CARTESIAN_POINT ( 'NONE',  ( -19.27153818831731158, 23.75761453444584248, -221.9111479746408975 ) ) ;
#1213 = CARTESIAN_POINT ( 'NONE',  ( 22.05207439088920651, 1.190718621721708947, -218.4927357815377604 ) ) ;
#1214 = CARTESIAN_POINT ( 'NONE',  ( -23.70785736019170997, 7.942585827099451379, -6.110416780456437991 ) ) ;
#1215 = CARTESIAN_POINT ( 'NONE',  ( 19.81239090451984097, -2.079411191919079638, -222.8294590615037123 ) ) ;
#1216 = DIRECTION ( 'NONE',  ( 0.000000000000000000, 0.000000000000000000, -1.000000000000000000 ) ) ;
#1217 = CARTESIAN_POINT ( 'NONE',  ( 23.48259192634075632, -8.786327662478353062, -220.0176983167915807 ) ) ;
#1218 = CARTESIAN_POINT ( 'NONE',  ( -16.76449091996730090, -6.021196472930381738, -231.5810252088758432 ) ) ;
#1219 = CARTESIAN_POINT ( 'NONE',  ( -22.17907062223998338, -6.115498295305363818, 7.938811080418386013 ) ) ;
#1220 = DIRECTION ( 'NONE',  ( -1.000000000000000000, 0.000000000000000000, 0.000000000000000000 ) ) ;
#1221 = CARTESIAN_POINT ( 'NONE',  ( -8.894613172508529786, 25.42460746921206294, -232.3150764041658363 ) ) ;
#1222 = CARTESIAN_POINT ( 'NONE',  ( 12.79824285610881063, -25.13061632922516253, -232.1172912921500426 ) ) ;
#1223 = AXIS2_PLACEMENT_3D ( 'NONE', #21571, #2886, #14628 ) ;
#1224 = CARTESIAN_POINT ( 'NONE',  ( 26.54225689383817866, -6.924125931238839016, -230.1506921200174247 ) ) ;
#1225 = CARTESIAN_POINT ( 'NONE',  ( -13.96147744945181124, 5.260363697127891314, -222.3342733685200301 ) ) ;
#1226 = CARTESIAN_POINT ( 'NONE',  ( -17.72669652144150376, 1.460525322529694581, -220.6883622781615202 ) ) ;
#1227 = CARTESIAN_POINT ( 'NONE',  ( 14.73597170006453361, 7.272367905564328439, -221.0092474305599239 ) ) ;
#1228 = AXIS2_PLACEMENT_3D ( 'NONE', #8171, #4772, #4997 ) ;
#1229 = CARTESIAN_POINT ( 'NONE',  ( -0.8455829679720252567, -23.09678443543459991, -232.4899849032512122 ) ) ;
#1230 = CARTESIAN_POINT ( 'NONE',  ( 15.01439307471096463, 1.118969480519667048, -226.7488225241675366 ) ) ;
#1231 = CARTESIAN_POINT ( 'NONE',  ( -20.87212828950092813, -0.8819659211619411687, -215.0000000018925448 ) ) ;
#1232 = CARTESIAN_POINT ( 'NONE',  ( 15.23494377589453919, 15.24947835004434538, -215.7641128510430519 ) ) ;
#1233 = CARTESIAN_POINT ( 'NONE',  ( 1.557078628722260438, 24.20011951319323273, -235.1441088220640268 ) ) ;
#1234 = CARTESIAN_POINT ( 'NONE',  ( 16.50219604690516206, -6.005650786285340104, -230.9082164827931933 ) ) ;
#1235 = CARTESIAN_POINT ( 'NONE',  ( -14.73016414256368911, 22.23431809695627237, -217.1425123644553707 ) ) ;
#1236 = CARTESIAN_POINT ( 'NONE',  ( -28.13472254077564116, 12.33996625515159629, -224.9141344439281909 ) ) ;
#1237 = EDGE_CURVE ( 'NONE', #12803, #17859, #13371, .T. ) ;
#1238 = CARTESIAN_POINT ( 'NONE',  ( 8.865150807857233417, 8.939496441981303221, -220.7647208555746090 ) ) ;
#1239 = CARTESIAN_POINT ( 'NONE',  ( -27.56397725925346975, 4.259055856374357241, -222.4951663284069241 ) ) ;
#1240 = CARTESIAN_POINT ( 'NONE',  ( -3.673551555920188783, 29.81207051619892923, -228.8770490300152005 ) ) ;
#1241 = AXIS2_PLACEMENT_3D ( 'NONE', #3863, #17832, #14871 ) ;
#1242 = CARTESIAN_POINT ( 'NONE',  ( 25.33562512631297281, 12.25422971834577268, -228.6777356031426791 ) ) ;
#1243 = CARTESIAN_POINT ( 'NONE',  ( 7.067550969709256670, 17.75197616922148569, -219.3387126207321955 ) ) ;
#1244 = CARTESIAN_POINT ( 'NONE',  ( 15.05575868828727515, -2.428864548505686560, -227.9368649688638584 ) ) ;
#1245 = CARTESIAN_POINT ( 'NONE',  ( 10.76794919243112325, 1.318693451189210089E-15, 93.00000000000000000 ) ) ;
#1246 = CARTESIAN_POINT ( 'NONE',  ( -26.43144772945995413, -6.745116643720071359, -219.5134289301136050 ) ) ;
#1247 = CARTESIAN_POINT ( 'NONE',  ( 14.68783945462866924, 9.535285537539673228, -219.4694094309942045 ) ) ;
#1248 = CARTESIAN_POINT ( 'NONE',  ( -2.827720241434194648, -28.87017495157254743, -218.9856045314649577 ) ) ;
#1249 = CARTESIAN_POINT ( 'NONE',  ( 18.77064933249683065, 2.992341472042430173, -225.2461773443920663 ) ) ;
#1250 = CARTESIAN_POINT ( 'NONE',  ( -10.32994309255856535, 16.55762392127841665, -218.3313395458419279 ) ) ;
#1251 = CARTESIAN_POINT ( 'NONE',  ( 11.63416633096549369, -11.60453582225250990, -230.7583135875248104 ) ) ;
#1252 = CARTESIAN_POINT ( 'NONE',  ( 12.79953165872901266, 10.20044330008568778, -230.3912386799665626 ) ) ;
#1253 = CARTESIAN_POINT ( 'NONE',  ( -4.080659539198054020, 15.43130099126780408, -228.8058965243247656 ) ) ;
#1254 = CARTESIAN_POINT ( 'NONE',  ( -17.58289524052909414, 0.7988212499981205417, -233.9567931471624149 ) ) ;
#1255 = CARTESIAN_POINT ( 'NONE',  ( -23.46219451118877330, -13.03948552059806509, -221.3852197888554372 ) ) ;
#1256 = CARTESIAN_POINT ( 'NONE',  ( 28.77543668145700195, 2.466904630248945907, -219.6646827587300947 ) ) ;
#1257 = AXIS2_PLACEMENT_3D ( 'NONE', #13932, #6948, #13820 ) ;
#1258 = CARTESIAN_POINT ( 'NONE',  ( 0.000000000000000000, -23.00000000000006040, -55.00000000000000000 ) ) ;
#1259 = CARTESIAN_POINT ( 'NONE',  ( -23.85689329484546661, -4.322701801676343436, -216.0188046937498996 ) ) ;
#1260 = CARTESIAN_POINT ( 'NONE',  ( 23.18902850759750933, 20.27908137164207147, -226.2847847834817117 ) ) ;
#1261 = CARTESIAN_POINT ( 'NONE',  ( -26.04932551096112192, 5.001193774903864409, -228.9498367494266802 ) ) ;
#1262 = CARTESIAN_POINT ( 'NONE',  ( 2.291262277241625345, 17.20278591336981222, -216.2185160402476924 ) ) ;
#1263 = CARTESIAN_POINT ( 'NONE',  ( 7.803634760976553508, 10.78293796201124266, -229.6314106675118865 ) ) ;
#1264 = EDGE_CURVE ( 'NONE', #8552, #15629, #3655, .T. ) ;
#1265 = CARTESIAN_POINT ( 'NONE',  ( -3.786803964513834941, -14.74062382431161566, -229.2965385003435586 ) ) ;
#1266 = VERTEX_POINT ( 'NONE', #12280 ) ;
#1267 = CARTESIAN_POINT ( 'NONE',  ( 2.283233934795953601, -16.37150177406293849, -220.5471140349473842 ) ) ;
#1268 = CARTESIAN_POINT ( 'NONE',  ( -11.89542918462869103, -0.2773029175206048191, -224.4556830488584467 ) ) ;
#1269 = CARTESIAN_POINT ( 'NONE',  ( 14.31589812732703670, -5.349901619299376243, -221.2752230612865105 ) ) ;
#1270 = CARTESIAN_POINT ( 'NONE',  ( -20.85586116824185510, -1.996934699305910499, -232.3804859832740135 ) ) ;
#1271 = AXIS2_PLACEMENT_3D ( 'NONE', #9116, #20803, #5381 ) ;
#1272 = CARTESIAN_POINT ( 'NONE',  ( -13.33530847390368024, -5.065163879519744228, -226.5386329521395226 ) ) ;
#1273 = AXIS2_PLACEMENT_3D ( 'NONE', #3060, #20052, #18498 ) ;
#1274 = CARTESIAN_POINT ( 'NONE',  ( 10.59524789654300925, 9.532374763983630928, -223.0758647391057821 ) ) ;
#1275 = FACE_OUTER_BOUND ( 'NONE', #18605, .T. ) ;
#1276 = CARTESIAN_POINT ( 'NONE',  ( -21.12280458060320498, 13.61074013710079988, -216.5529903464332335 ) ) ;
#1277 = CARTESIAN_POINT ( 'NONE',  ( 12.14863411169100971, 10.95505907656739097, -219.3725293661985063 ) ) ;
#1278 = CARTESIAN_POINT ( 'NONE',  ( 12.04687593227112430, 27.54339840196571743, -224.6466266724203820 ) ) ;
#1279 = CARTESIAN_POINT ( 'NONE',  ( 13.50603691942335693, 22.79443449215731832, -229.7689193854997995 ) ) ;
#1280 = CARTESIAN_POINT ( 'NONE',  ( 15.81704710165450756, -18.55181613945514840, -214.8869746720286287 ) ) ;
#1281 = CARTESIAN_POINT ( 'NONE',  ( -9.982417347796181062, 8.907629238417765549, -225.5124013436514474 ) ) ;
#1282 = CARTESIAN_POINT ( 'NONE',  ( -5.566280468132954518, 29.91920859341914962, -222.2705790733167817 ) ) ;
#1283 = CARTESIAN_POINT ( 'NONE',  ( -19.75205891382245227, -22.10994567413457546, -223.7241504221178729 ) ) ;
#1284 = CARTESIAN_POINT ( 'NONE',  ( -17.96792326766206926, -0.6237852504629022299, -217.9759415197746932 ) ) ;
#1285 = CARTESIAN_POINT ( 'NONE',  ( -17.50000000000000355, 2.143131898507868643E-15, -70.00000000000000000 ) ) ;
#1286 = CARTESIAN_POINT ( 'NONE',  ( 22.66390650824515873, 11.48342577402021725, -231.3155567808436217 ) ) ;
#1287 = CARTESIAN_POINT ( 'NONE',  ( 15.27128302093890255, -22.10320814337061535, -229.9052109820655119 ) ) ;
#1288 = CARTESIAN_POINT ( 'NONE',  ( -21.23733589435050817, 17.25275849955597351, -229.9547908233139708 ) ) ;
#1289 = CIRCLE ( 'NONE', #225, 21.50000000000000711 ) ;
#1290 = CARTESIAN_POINT ( 'NONE',  ( -21.28605893225895684, -20.43870967537180050, -221.0356759888913700 ) ) ;
#1291 = CARTESIAN_POINT ( 'NONE',  ( -19.11923763334766946, 1.257783214997954202, -219.7591028439344711 ) ) ;
#1292 = CARTESIAN_POINT ( 'NONE',  ( 12.58577552758108986, 11.40439409249366420, -217.4478085440898951 ) ) ;
#1293 = EDGE_LOOP ( 'NONE', ( #4845, #14996, #17881, #4341 ) ) ;
#1294 = CARTESIAN_POINT ( 'NONE',  ( 3.763426558366607111, 28.60172112197566818, -230.1816715025297526 ) ) ;
#1295 = CARTESIAN_POINT ( 'NONE',  ( -26.47652094774193188, -8.527600130219385122, -218.5932275281782324 ) ) ;
#1296 = CARTESIAN_POINT ( 'NONE',  ( -24.87076642133107995, -2.621478783564629378, 9.673133369187967290 ) ) ;
#1297 = DIRECTION ( 'NONE',  ( -2.891205793294678696E-17, 0.000000000000000000, -1.000000000000000000 ) ) ;
#1298 = CARTESIAN_POINT ( 'NONE',  ( -3.003186468682855104, 15.63968344752823469, -231.5301608670590667 ) ) ;
#1299 = CARTESIAN_POINT ( 'NONE',  ( -17.24073315697368969, -20.31883122441189826, -234.2947248507418863 ) ) ;
#1300 = CARTESIAN_POINT ( 'NONE',  ( 2.378655016347637652, -14.31292064579845302, -219.9942319014987220 ) ) ;
#1301 = CARTESIAN_POINT ( 'NONE',  ( 22.14341918773124362, -7.622004812940091689, -217.4502831791021720 ) ) ;
#1302 = CARTESIAN_POINT ( 'NONE',  ( -10.30040261405712698, 19.75576125044891285, -218.0811964201226658 ) ) ;
#1303 = CARTESIAN_POINT ( 'NONE',  ( 10.90137817157632227, 16.64712710991609868, -230.5401786220292593 ) ) ;
#1304 = CYLINDRICAL_SURFACE ( 'NONE', #3314, 3.000000000000002665 ) ;
#1305 = CARTESIAN_POINT ( 'NONE',  ( -21.75607741976026333, 20.26169853110213381, -228.4128163609909450 ) ) ;
#1306 = CARTESIAN_POINT ( 'NONE',  ( -15.14636561941736481, -8.091785236158230532, -228.8632199501622608 ) ) ;
#1307 = VECTOR ( 'NONE', #17008, 1000.000000000000000 ) ;
#1308 = CARTESIAN_POINT ( 'NONE',  ( -14.87932799058895128, 18.71706570923887369, -231.8731726670167745 ) ) ;
#1309 = CARTESIAN_POINT ( 'NONE',  ( 26.28575214971901630, 3.591103948354015696, -217.0994821834097763 ) ) ;
#1310 = CARTESIAN_POINT ( 'NONE',  ( -5.529079411693809121, 13.00503897727793401, -226.8014833675713646 ) ) ;
#1311 = ADVANCED_FACE ( 'NONE', ( #17464 ), #8333, .T. ) ;
#1312 = CARTESIAN_POINT ( 'NONE',  ( 17.93010821528303822, -10.80507700282924688, -233.3968735006674251 ) ) ;
#1313 = CARTESIAN_POINT ( 'NONE',  ( 0.000000000000000000, 23.00000000000000000, -69.99999999999998579 ) ) ;
#1314 = EDGE_LOOP ( 'NONE', ( #1892, #17605, #13463, #18308 ) ) ;
#1315 = CARTESIAN_POINT ( 'NONE',  ( -17.39699619235753048, 15.64332637722790054, -216.0406373264262641 ) ) ;
#1316 = CARTESIAN_POINT ( 'NONE',  ( -7.243062456665192883, -20.67674855546218637, -233.5126394780404553 ) ) ;
#1317 = FACE_OUTER_BOUND ( 'NONE', #4433, .T. ) ;
#1318 = CARTESIAN_POINT ( 'NONE',  ( 4.907833106823921376, 13.98151846258800290, -229.0190609869640923 ) ) ;
#1319 = CARTESIAN_POINT ( 'NONE',  ( -2.775557561562891351E-14, 0.000000000000000000, -105.0000000000000142 ) ) ;
#1320 = PRODUCT_DEFINITION_CONTEXT ( 'detailed design', #3384, 'design' ) ;
#1321 = CARTESIAN_POINT ( 'NONE',  ( 19.06763123184207487, -2.048228142369658666, -218.2337357994572073 ) ) ;
#1322 = FILL_AREA_STYLE_COLOUR ( '', #5562 ) ;
#1323 = CARTESIAN_POINT ( 'NONE',  ( -28.17543631911187063, 3.557555778861649642, -230.1980773687482156 ) ) ;
#1324 = CARTESIAN_POINT ( 'NONE',  ( -17.94782256308196366, 19.07396065564992682, -232.7143578890335220 ) ) ;
#1325 = CARTESIAN_POINT ( 'NONE',  ( 14.21126657910812874, 6.833562750302326627, -220.2783117037562874 ) ) ;
#1326 = CARTESIAN_POINT ( 'NONE',  ( 14.45550103314422508, 0.1264054796715357587, -222.0026434553262504 ) ) ;
#1327 = CARTESIAN_POINT ( 'NONE',  ( 22.00000000000000000, 0.000000000000000000, -221.9999999999999716 ) ) ;
#1328 = FACE_OUTER_BOUND ( 'NONE', #7121, .T. ) ;
#1329 = CARTESIAN_POINT ( 'NONE',  ( 26.42227051273691885, -8.869064526452445918, -225.3570890864022260 ) ) ;
#1330 = CARTESIAN_POINT ( 'NONE',  ( -22.23616899077527975, -11.51447210886970751, -217.5950109096934568 ) ) ;
#1331 = CARTESIAN_POINT ( 'NONE',  ( -22.56784948551151615, -4.447299220502048733, 8.962591915120089681 ) ) ;
#1332 = CARTESIAN_POINT ( 'NONE',  ( -19.63401512838747820, 0.000000000000000000, 77.51594804401857175 ) ) ;
#1333 = CARTESIAN_POINT ( 'NONE',  ( 8.250760074138732136, 14.96691001493985951, -221.7548416114337613 ) ) ;
#1334 = CARTESIAN_POINT ( 'NONE',  ( 8.477993572791891808, -8.340333012420144243, -224.9486226631276793 ) ) ;
#1335 = CARTESIAN_POINT ( 'NONE',  ( 6.741123954526870854, -14.00899218320067341, -219.0418835583997179 ) ) ;
#1336 = ORIENTED_EDGE ( 'NONE', *, *, #14070, .F. ) ;
#1337 = CARTESIAN_POINT ( 'NONE',  ( -9.954421844142357756, 11.21484508112568079, -226.0177122452137439 ) ) ;
#1338 = CARTESIAN_POINT ( 'NONE',  ( 17.22423229049764970, 1.395540479540137380, -217.3898520248025363 ) ) ;
#1339 = CARTESIAN_POINT ( 'NONE',  ( 22.37742875470728876, 11.29804624588327577, -218.9256858961603882 ) ) ;
#1340 = CARTESIAN_POINT ( 'NONE',  ( -7.719684133369767665, -19.28933804209621528, -218.9187502689394478 ) ) ;
#1341 = CARTESIAN_POINT ( 'NONE',  ( -14.49943138577569535, 0.2467007162552621036, 93.00000000000002842 ) ) ;
#1342 = CARTESIAN_POINT ( 'NONE',  ( -11.10150084103673684, 3.549415896002023896, -226.0408865487038952 ) ) ;
#1343 = EDGE_LOOP ( 'NONE', ( #18591, #20601, #5350, #21894 ) ) ;
#1344 = CARTESIAN_POINT ( 'NONE',  ( 4.228809304811371739, 12.93497549386982470, -230.7917784105561907 ) ) ;
#1345 = CARTESIAN_POINT ( 'NONE',  ( -0.4465333940385243228, 12.27026616490476485, -221.3722328744566425 ) ) ;
#1346 = CARTESIAN_POINT ( 'NONE',  ( 15.06969459085678942, -9.685035337269850331, -230.1890524597188801 ) ) ;
#1347 = CARTESIAN_POINT ( 'NONE',  ( -11.69688825528096388, 18.63404371591177622, -215.8612738028812714 ) ) ;
#1348 = CARTESIAN_POINT ( 'NONE',  ( -13.56774755469388616, 7.311522441667196226, -219.1912666243428021 ) ) ;
#1349 = CARTESIAN_POINT ( 'NONE',  ( 3.137667653003819446, 15.44806861187908176, -232.6841782316817842 ) ) ;
#1350 = CARTESIAN_POINT ( 'NONE',  ( -16.66929017373293931, 3.065794289431343689, -220.7800282905443794 ) ) ;
#1351 = CARTESIAN_POINT ( 'NONE',  ( -3.082945806077231676, 30.69897765966285874, -224.2387254578930822 ) ) ;
#1352 = CARTESIAN_POINT ( 'NONE',  ( 19.20300624114736721, 0.6066039755357417462, -231.5046416827383950 ) ) ;
#1353 = CARTESIAN_POINT ( 'NONE',  ( 12.83388873239664996, 22.07510045760132655, -230.4740059944613222 ) ) ;
#1354 = CARTESIAN_POINT ( 'NONE',  ( 24.56541673123750158, -5.996287403333383281, -231.6940117905984664 ) ) ;
#1355 = LINE ( 'NONE', #3251, #13869 ) ;
#1356 = CARTESIAN_POINT ( 'NONE',  ( -28.87859926594958537, -0.8320174534291842061, -222.6356913548140142 ) ) ;
#1357 = CARTESIAN_POINT ( 'NONE',  ( 14.80394259695730064, 1.224172658189580432, -225.4564070658925061 ) ) ;
#1358 = CARTESIAN_POINT ( 'NONE',  ( -20.91998163778511355, -19.58520498255836628, -224.2692832511962990 ) ) ;
#1359 = CARTESIAN_POINT ( 'NONE',  ( 20.28602808787860567, 1.649471991126377768, -227.5337793182429493 ) ) ;
#1360 = CARTESIAN_POINT ( 'NONE',  ( -12.78923236353123727, 15.53885160143439315, -231.8946633672937878 ) ) ;
#1361 = CARTESIAN_POINT ( 'NONE',  ( 21.28562020585086501, -15.94148943779260819, -218.1725164024425396 ) ) ;
#1362 = CARTESIAN_POINT ( 'NONE',  ( 11.83256327006771969, 5.988634687709346593, -225.8999299265561831 ) ) ;
#1363 = CARTESIAN_POINT ( 'NONE',  ( -17.14223598032838325, 23.31797360549976261, -226.5771676936548431 ) ) ;
#1364 = CARTESIAN_POINT ( 'NONE',  ( -7.834600152078401436, 27.83486203824852012, -220.1209588485844222 ) ) ;
#1365 = VERTEX_POINT ( 'NONE', #2034 ) ;
#1366 = CARTESIAN_POINT ( 'NONE',  ( -13.13215111221786024, -8.938624195428067409, -226.3235457059856515 ) ) ;
#1367 = CARTESIAN_POINT ( 'NONE',  ( 20.09685469220202236, -2.033783885649083079, -233.1448060988079760 ) ) ;
#1368 = CARTESIAN_POINT ( 'NONE',  ( 0.000000000000000000, 0.000000000000000000, -100.7764571353075524 ) ) ;
#1369 = CARTESIAN_POINT ( 'NONE',  ( -28.08095947817005822, 1.343466879924336999, -219.1986237337335695 ) ) ;
#1370 = CARTESIAN_POINT ( 'NONE',  ( 5.702651035983461902, 12.42242820409033222, -224.7304266323218656 ) ) ;
#1371 = CARTESIAN_POINT ( 'NONE',  ( -17.29038495093124084, 2.707785585324113065, -229.0475017805649998 ) ) ;
#1372 = CARTESIAN_POINT ( 'NONE',  ( 2.000982021813747291, 12.72833461843010205, -228.3416607300594308 ) ) ;
#1373 = CARTESIAN_POINT ( 'NONE',  ( 17.76485367938521875, 4.373152267827974171, -218.8623009891758215 ) ) ;
#1374 = CARTESIAN_POINT ( 'NONE',  ( -8.731539701382653007, -8.828156491469059119, -227.3463890218280596 ) ) ;
#1375 = ORIENTED_EDGE ( 'NONE', *, *, #1141, .T. ) ;
#1376 = CARTESIAN_POINT ( 'NONE',  ( -17.81508947870519322, -18.77243306401324219, -218.1930932538018340 ) ) ;
#1377 = AXIS2_PLACEMENT_3D ( 'NONE', #15606, #297, #5573 ) ;
#1378 = CARTESIAN_POINT ( 'NONE',  ( -27.53108621362071773, 14.15137273650544536, -219.7961709676081625 ) ) ;
#1379 = CARTESIAN_POINT ( 'NONE',  ( 8.257114973007913861, -25.39836461225790742, -232.6217252414676295 ) ) ;
#1380 = CARTESIAN_POINT ( 'NONE',  ( 26.60633779560760459, -14.33430814915920593, -230.5388497754989885 ) ) ;
#1381 = CARTESIAN_POINT ( 'NONE',  ( -16.76449091996730090, -6.021196472930381738, -231.5810252088758432 ) ) ;
#1382 =( REPRESENTATION_RELATIONSHIP ('NONE','NONE', #5277, #3834 ) REPRESENTATION_RELATIONSHIP_WITH_TRANSFORMATION ( #6460 )SHAPE_REPRESENTATION_RELATIONSHIP( ) );
#1383 = CARTESIAN_POINT ( 'NONE',  ( 20.40268796714816801, 18.65534563792085621, -219.5587498978784993 ) ) ;
#1384 = CARTESIAN_POINT ( 'NONE',  ( 1.526556658859591000E-13, -22.63401512838754570, 77.51594804401857175 ) ) ;
#1385 = CARTESIAN_POINT ( 'NONE',  ( -21.29946384424354733, 21.01772963953914442, -222.5871995662667757 ) ) ;
#1386 = CARTESIAN_POINT ( 'NONE',  ( 9.575488824002899690, 13.89846378187365694, -220.1158735840035945 ) ) ;
#1387 = CARTESIAN_POINT ( 'NONE',  ( 17.43816562714825125, 15.15720016074785903, -232.3748236813696906 ) ) ;
#1388 = CARTESIAN_POINT ( 'NONE',  ( 21.46274988498219471, 20.25395488059580984, -223.1777011585387243 ) ) ;
#1389 = CARTESIAN_POINT ( 'NONE',  ( 10.56186985702850833, -7.684747726859879613, -229.4341029534429026 ) ) ;
#1390 = CARTESIAN_POINT ( 'NONE',  ( -10.24168223636446662, 16.14271751156598356, -231.4847994864913971 ) ) ;
#1391 = CARTESIAN_POINT ( 'NONE',  ( -28.99926036811508467, 3.909990568804979194, -228.9613767892386988 ) ) ;
#1392 = DIRECTION ( 'NONE',  ( 0.000000000000000000, 0.000000000000000000, -1.000000000000000000 ) ) ;
#1393 = ADVANCED_FACE ( 'NONE', ( #19248 ), #3828, .T. ) ;
#1394 = CARTESIAN_POINT ( 'NONE',  ( 11.62313423782632782, 11.98467543564608029, -219.7293303032897995 ) ) ;
#1395 = CARTESIAN_POINT ( 'NONE',  ( 5.240643865192946116, -17.54789557311951143, -217.3772572127879812 ) ) ;
#1396 = CARTESIAN_POINT ( 'NONE',  ( -14.94640692938030746, 5.382918922058764544, -220.5478552936960455 ) ) ;
#1397 = VECTOR ( 'NONE', #13022, 1000.000000000000000 ) ;
#1398 = CARTESIAN_POINT ( 'NONE',  ( 10.25948093768852054, 28.38842464930171872, -224.3436940787075855 ) ) ;
#1399 = CARTESIAN_POINT ( 'NONE',  ( -16.76449091996730090, -6.021196472930381738, -231.5810252088758432 ) ) ;
#1400 = CARTESIAN_POINT ( 'NONE',  ( 12.23284375931666013, 4.108221165122169616, -224.0993108960438462 ) ) ;
#1401 = CARTESIAN_POINT ( 'NONE',  ( 7.116434306140963173, 9.967665124511082553, -224.4990387090310833 ) ) ;
#1402 = ORIENTED_EDGE ( 'NONE', *, *, #13977, .F. ) ;
#1403 = CARTESIAN_POINT ( 'NONE',  ( -10.84997096467605182, 25.01800101807719301, -232.4518260228253155 ) ) ;
#1404 = CARTESIAN_POINT ( 'NONE',  ( 15.15335612453267089, -12.60200553607942098, -219.4566848265094166 ) ) ;
#1405 = CARTESIAN_POINT ( 'NONE',  ( 28.46281617689634302, -10.50803404096709137, -222.5507679334694728 ) ) ;
#1406 = CARTESIAN_POINT ( 'NONE',  ( 0.000000000000000000, -25.00000000000000000, 75.00000000000000000 ) ) ;
#1407 = CARTESIAN_POINT ( 'NONE',  ( 4.656903975822286768, 13.45000048768594780, -227.6722060245555497 ) ) ;
#1408 = CARTESIAN_POINT ( 'NONE',  ( -15.80613518906033121, -10.93105391054944597, -234.9065563738643903 ) ) ;
#1409 = CARTESIAN_POINT ( 'NONE',  ( 7.437838793555467731, -20.85539581353325289, -233.9154700400843865 ) ) ;
#1410 = CARTESIAN_POINT ( 'NONE',  ( 11.90144651507291051, -8.898305237537579515, -228.5592478859710184 ) ) ;
#1411 = CARTESIAN_POINT ( 'NONE',  ( -8.112279890008961658, 11.99566605360304727, -225.9834628568286519 ) ) ;
#1412 = CARTESIAN_POINT ( 'NONE',  ( 12.91443243054181700, 13.28840485332751875, -229.6651346406987955 ) ) ;
#1413 = CARTESIAN_POINT ( 'NONE',  ( -16.15126510923403202, -0.4755054218165427615, -219.3066569788202571 ) ) ;
#1414 = CARTESIAN_POINT ( 'NONE',  ( -23.49520248890869212, 11.82830312093803649, -233.3871405502527807 ) ) ;
#1415 = CARTESIAN_POINT ( 'NONE',  ( -18.22136682449241363, -9.036057809225649606, -231.1742889867359736 ) ) ;
#1416 = ORIENTED_EDGE ( 'NONE', *, *, #4968, .F. ) ;
#1417 = CARTESIAN_POINT ( 'NONE',  ( -8.435479365662203577, 14.12888021429238528, -220.5365774424437859 ) ) ;
#1418 = CARTESIAN_POINT ( 'NONE',  ( 13.86383614057800884, 4.939477956453596441, -219.6543243356308324 ) ) ;
#1419 = CARTESIAN_POINT ( 'NONE',  ( -3.712761995161701911, 23.50704853188985766, -216.1220552374512067 ) ) ;
#1420 = CARTESIAN_POINT ( 'NONE',  ( 12.99512476935412231, -3.120572961704727977, -223.7636045402963987 ) ) ;
#1421 = CARTESIAN_POINT ( 'NONE',  ( -17.50000000000000711, 0.000000000000000000, -24.99999999999999645 ) ) ;
#1422 = VERTEX_POINT ( 'NONE', #7666 ) ;
#1423 = EDGE_CURVE ( 'NONE', #10960, #18642, #18111, .T. ) ;
#1424 = CARTESIAN_POINT ( 'NONE',  ( -18.70100282803782576, 16.58357028540773115, -216.4425743468854080 ) ) ;
#1425 = CARTESIAN_POINT ( 'NONE',  ( -11.51027863121307782, -1.790843358437596677, -225.0773512427349203 ) ) ;
#1426 = DIRECTION ( 'NONE',  ( -2.162300680179986877E-16, -1.000000000000000000, 0.000000000000000000 ) ) ;
#1427 = CARTESIAN_POINT ( 'NONE',  ( 12.10245006109274080, 26.02147364279441888, -220.6079829738538649 ) ) ;
#1428 = PLANE ( 'NONE',  #21312 ) ;
#1429 = CARTESIAN_POINT ( 'NONE',  ( 16.07085865561684201, -17.65509622858733252, -216.6880805489183501 ) ) ;
#1430 = PRESENTATION_STYLE_ASSIGNMENT (( #18544 ) ) ;
#1431 = CARTESIAN_POINT ( 'NONE',  ( -13.10651848559790444, 3.262242204071156948, -224.3513854875720597 ) ) ;
#1432 = CARTESIAN_POINT ( 'NONE',  ( -8.929606928624414408, 11.65278034267609186, -219.1999234847403386 ) ) ;
#1433 = CARTESIAN_POINT ( 'NONE',  ( 13.59483335902903178, 5.678732573479117640, -228.5032236586631313 ) ) ;
#1434 = CARTESIAN_POINT ( 'NONE',  ( -4.879290506874147226, -14.18937706998098136, -223.0759034783553147 ) ) ;
#1435 = CARTESIAN_POINT ( 'NONE',  ( -25.00000000000013500, 6.609496070381316956E-17, -10.00000000000000000 ) ) ;
#1436 = EDGE_CURVE ( 'NONE', #1916, #930, #572, .T. ) ;
#1437 = CARTESIAN_POINT ( 'NONE',  ( 25.18785298611088308, 3.974282393449815931, -218.7636041058819956 ) ) ;
#1438 = CARTESIAN_POINT ( 'NONE',  ( 28.08231343014353243, -2.974470402155979354, -225.4253119135968291 ) ) ;
#1439 = CARTESIAN_POINT ( 'NONE',  ( 14.35226977795134040, -1.892513177579410844, -227.3278729267533151 ) ) ;
#1440 = EDGE_CURVE ( 'NONE', #15541, #8028, #2581, .T. ) ;
#1441 = FACE_OUTER_BOUND ( 'NONE', #21298, .T. ) ;
#1442 = CARTESIAN_POINT ( 'NONE',  ( 1.455845656607152363E-13, -21.63401512838760610, -77.51594804401857175 ) ) ;
#1443 = CARTESIAN_POINT ( 'NONE',  ( 11.00580183749007190, 25.74996642444834904, -225.8602305833924788 ) ) ;
#1444 = ADVANCED_FACE ( 'NONE', ( #13058 ), #900, .F. ) ;
#1445 = CARTESIAN_POINT ( 'NONE',  ( 13.14132348467506439, -13.49276336982165780, -234.5843434792288633 ) ) ;
#1446 = CARTESIAN_POINT ( 'NONE',  ( 11.32394539683753720, -15.63383003174572572, -233.0723040138117881 ) ) ;
#1447 = CARTESIAN_POINT ( 'NONE',  ( -17.08384421609436643, 23.56421365837046622, -225.2902702884460666 ) ) ;
#1448 = CARTESIAN_POINT ( 'NONE',  ( 27.69955354773053458, 12.81264626165819287, -221.7750850138309602 ) ) ;
#1449 = CARTESIAN_POINT ( 'NONE',  ( 27.66944030902029539, 6.857614156517904291, -220.9860880211026313 ) ) ;
#1450 = CARTESIAN_POINT ( 'NONE',  ( -8.696851061449722309, -24.60219662023354914, -220.1357990587600852 ) ) ;
#1451 = CARTESIAN_POINT ( 'NONE',  ( 10.76794919243112325, 0.000000000000000000, 92.00000000000000000 ) ) ;
#1452 = CARTESIAN_POINT ( 'NONE',  ( -27.53108621362071773, 14.15137273650544536, -219.7961709676081625 ) ) ;
#1453 = CARTESIAN_POINT ( 'NONE',  ( 3.714886539878811789, 12.88803176524806560, -219.5889136906770034 ) ) ;
#1454 = CARTESIAN_POINT ( 'NONE',  ( 13.51502823286059929, -13.46037062290453790, -230.3041566501836144 ) ) ;
#1455 = CARTESIAN_POINT ( 'NONE',  ( 9.586902571418640662, 24.43292817174309661, -231.9968623198229807 ) ) ;
#1456 = CARTESIAN_POINT ( 'NONE',  ( -13.98136146596813845, 3.850743984385103680, -228.7620665878280590 ) ) ;
#1457 = CARTESIAN_POINT ( 'NONE',  ( 13.79814099039094089, 16.09927043668092850, -214.6489469124405502 ) ) ;
#1458 = CARTESIAN_POINT ( 'NONE',  ( -16.48591407464216729, 7.092323989942422635, -218.8909951703408012 ) ) ;
#1459 = CARTESIAN_POINT ( 'NONE',  ( -6.474151797443945533, 21.29193859232740138, -215.9573456447696458 ) ) ;
#1460 = CARTESIAN_POINT ( 'NONE',  ( 24.03642272140365677, 3.646960756862087205, -218.2320643939070806 ) ) ;
#1461 = CARTESIAN_POINT ( 'NONE',  ( 8.686008240521225332, 26.11221116136006515, -227.6539570933143466 ) ) ;
#1462 = CARTESIAN_POINT ( 'NONE',  ( 27.96460686140487084, -1.872811165202790340, -220.9791906660856000 ) ) ;
#1463 = FACE_OUTER_BOUND ( 'NONE', #17228, .T. ) ;
#1464 = CARTESIAN_POINT ( 'NONE',  ( 0.000000000000000000, 0.000000000000000000, 89.47905546699919910 ) ) ;
#1465 = CARTESIAN_POINT ( 'NONE',  ( -31.04415783139704388, 5.868882651865275690, -221.1472518903637194 ) ) ;
#1466 = CARTESIAN_POINT ( 'NONE',  ( -13.98007945013786291, -9.257046693524761949, -228.3752161438062842 ) ) ;
#1467 = CARTESIAN_POINT ( 'NONE',  ( 21.30611872263677498, 0.6836234283288439295, -227.9261315426025760 ) ) ;
#1468 = CARTESIAN_POINT ( 'NONE',  ( -14.94618804342693075, 22.09718979644185666, -219.6454806548149463 ) ) ;
#1469 =( NAMED_UNIT ( * ) PLANE_ANGLE_UNIT ( ) SI_UNIT ( $, .RADIAN. ) );
#1470 = CARTESIAN_POINT ( 'NONE',  ( 2.283233934795953601, -16.37150177406293849, -220.5471140349473842 ) ) ;
#1471 = CARTESIAN_POINT ( 'NONE',  ( 12.54860906168727652, 6.077542143275485031, -228.1605930327268368 ) ) ;
#1472 = CARTESIAN_POINT ( 'NONE',  ( -8.857704405076667342, 24.20848540845601704, -218.8859504303524091 ) ) ;
#1473 = CARTESIAN_POINT ( 'NONE',  ( -23.66836017558062011, 21.44695383684080525, -223.6245772351065568 ) ) ;
#1474 = ORIENTED_EDGE ( 'NONE', *, *, #16262, .T. ) ;
#1475 = CARTESIAN_POINT ( 'NONE',  ( 24.13177372007769961, -1.862525787088729956, -215.1116454360890202 ) ) ;
#1476 = ORIENTED_EDGE ( 'NONE', *, *, #15181, .T. ) ;
#1477 = CARTESIAN_POINT ( 'NONE',  ( 12.58590500897257947, 11.38573988265384607, -230.4867078522624695 ) ) ;
#1478 = CARTESIAN_POINT ( 'NONE',  ( -17.00265675087485917, 7.324244386240115645, -218.5600005870616656 ) ) ;
#1479 = CARTESIAN_POINT ( 'NONE',  ( -21.93223149637851677, 1.726402211042445067, -231.1052103444381203 ) ) ;
#1480 = DIRECTION ( 'NONE',  ( -6.123233995736766036E-17, 0.000000000000000000, 1.000000000000000000 ) ) ;
#1481 = CARTESIAN_POINT ( 'NONE',  ( -29.73963803141277396, -7.146848409970624871, -220.9878827551818858 ) ) ;
#1482 = CARTESIAN_POINT ( 'NONE',  ( 16.64575860537911112, 25.12688477742292648, -227.5050599151411745 ) ) ;
#1483 = CARTESIAN_POINT ( 'NONE',  ( -15.99768154740552717, 2.245235659047613908, -226.7015216759272107 ) ) ;
#1484 = CARTESIAN_POINT ( 'NONE',  ( -2.917590128672695293, 18.81591489065672818, -216.3635620530855022 ) ) ;
#1485 = CARTESIAN_POINT ( 'NONE',  ( 27.08994772491946890, 9.675875910685000747, -221.3471992134593336 ) ) ;
#1486 = CARTESIAN_POINT ( 'NONE',  ( -7.253640667752737414, -12.78251829042625687, -230.3353663933772282 ) ) ;
#1487 = ORIENTED_EDGE ( 'NONE', *, *, #6538, .F. ) ;
#1488 = CARTESIAN_POINT ( 'NONE',  ( -10.22552941266963877, -9.699191453761107695, -225.4315674810442545 ) ) ;
#1489 = CARTESIAN_POINT ( 'NONE',  ( -28.88770769694534479, 14.24820799418726480, -223.2044777450442155 ) ) ;
#1490 = CARTESIAN_POINT ( 'NONE',  ( 4.201723131641114328, -20.76291977712905279, -215.9522215885928347 ) ) ;
#1491 = CARTESIAN_POINT ( 'NONE',  ( -2.208416658185406334, 29.10348627872611615, -219.8480645685746424 ) ) ;
#1492 = CARTESIAN_POINT ( 'NONE',  ( 14.87770435525805013, -9.987123395515542512, -215.8225415630120665 ) ) ;
#1493 = CARTESIAN_POINT ( 'NONE',  ( -20.18470553695442860, -13.13924840112635195, -232.9662461559857718 ) ) ;
#1494 = CARTESIAN_POINT ( 'NONE',  ( 16.82251835652528982, 18.18719385133374544, -231.8032941011735772 ) ) ;
#1495 = CARTESIAN_POINT ( 'NONE',  ( -10.46043650402819125, 8.998596506756641134, -222.4402691847174083 ) ) ;
#1496 = CARTESIAN_POINT ( 'NONE',  ( 8.778334628954494789, 12.71782457734010841, -222.1923057070808909 ) ) ;
#1497 = AXIS2_PLACEMENT_3D ( 'NONE', #10710, #17575, #21149 ) ;
#1498 = CARTESIAN_POINT ( 'NONE',  ( 14.39473142419577023, 15.98257177912839389, -217.4557725731239373 ) ) ;
#1499 = CARTESIAN_POINT ( 'NONE',  ( 9.094331215210646135, 23.85463374792894342, -219.7669638091879847 ) ) ;
#1500 = CARTESIAN_POINT ( 'NONE',  ( 5.982199551433209805, -30.67818700677413091, -221.2919386232889849 ) ) ;
#1501 = CARTESIAN_POINT ( 'NONE',  ( -13.06839468023815165, 25.32320678245788059, -229.0099538679170053 ) ) ;
#1502 = PRODUCT_DEFINITION_SHAPE ( 'NONE', 'NONE',  #22266 ) ;
#1503 = DIRECTION ( 'NONE',  ( -0.000000000000000000, -0.000000000000000000, -1.000000000000000000 ) ) ;
#1504 = CARTESIAN_POINT ( 'NONE',  ( -25.00000000000010303, 0.000000000000000000, 75.00000000000000000 ) ) ;
#1505 = AXIS2_PLACEMENT_3D ( 'NONE', #2740, #9620, #3068 ) ;
#1506 = CARTESIAN_POINT ( 'NONE',  ( 8.990474075060864934, -28.03008174514034678, -221.5310560963409330 ) ) ;
#1507 = CARTESIAN_POINT ( 'NONE',  ( -23.20103936322198024, 10.64725167743880085, -231.7714206262400864 ) ) ;
#1508 = CARTESIAN_POINT ( 'NONE',  ( -1.038524475621362075, 14.89017051181998141, -222.3948816610352139 ) ) ;
#1509 = EDGE_CURVE ( 'NONE', #11033, #10050, #11370, .T. ) ;
#1510 = CARTESIAN_POINT ( 'NONE',  ( -24.15031621174628285, -13.05338392360020627, -219.0842748323915714 ) ) ;
#1511 = CARTESIAN_POINT ( 'NONE',  ( -17.29038495093124084, 2.707785585324113065, -229.0475017805649998 ) ) ;
#1512 = CIRCLE ( 'NONE', #3297, 17.50000000000007816 ) ;
#1513 = CARTESIAN_POINT ( 'NONE',  ( 13.06625079052675531, 10.14096931681969238, -232.1435240729728093 ) ) ;
#1514 = ORIENTED_EDGE ( 'NONE', *, *, #6789, .T. ) ;
#1515 = CARTESIAN_POINT ( 'NONE',  ( -7.825349071214003693, 24.14595706726266755, -216.5959661901539732 ) ) ;
#1516 = CARTESIAN_POINT ( 'NONE',  ( 11.99204520814221553, -11.76515119196726467, -228.0494177468141572 ) ) ;
#1517 = CARTESIAN_POINT ( 'NONE',  ( 20.33239098169031323, -9.013719117183370599, -216.4483480702011775 ) ) ;
#1518 = CARTESIAN_POINT ( 'NONE',  ( -12.50000000000000355, 1.530808498934191916E-15, -25.00000000000000000 ) ) ;
#1519 = CARTESIAN_POINT ( 'NONE',  ( 4.354034006296288339, 14.09944204372416188, -221.2519525881239417 ) ) ;
#1520 = CARTESIAN_POINT ( 'NONE',  ( -10.37549270978917448, -7.969494006339708392, -220.1790165754723603 ) ) ;
#1521 = CARTESIAN_POINT ( 'NONE',  ( -14.34280792637948743, -22.10828917559366147, -217.4172704053049756 ) ) ;
#1522 = CARTESIAN_POINT ( 'NONE',  ( 12.73130673999417795, -23.76414828096303467, -217.7386337832039942 ) ) ;
#1523 = CARTESIAN_POINT ( 'NONE',  ( -11.11479000491124047, 20.76372272540567110, -218.2001872134434564 ) ) ;
#1524 = CARTESIAN_POINT ( 'NONE',  ( 7.951191770265756631, 20.55701948568933091, -231.2149185317973661 ) ) ;
#1525 = CARTESIAN_POINT ( 'NONE',  ( -21.02719846458807851, 18.12262440796364871, -218.0220709499931502 ) ) ;
#1526 = CARTESIAN_POINT ( 'NONE',  ( -24.69837543585720141, 12.57569301576483589, -232.4521327773205428 ) ) ;
#1527 = CARTESIAN_POINT ( 'NONE',  ( -24.95561420934758701, -9.148537957313763513, -219.7769960911953149 ) ) ;
#1528 = ORIENTED_EDGE ( 'NONE', *, *, #6345, .F. ) ;
#1529 = CIRCLE ( 'NONE', #7295, 20.99999999999999645 ) ;
#1530 = CARTESIAN_POINT ( 'NONE',  ( -8.317278876689359279, 23.15034512777772235, -218.2935523245793092 ) ) ;
#1531 = CARTESIAN_POINT ( 'NONE',  ( 16.21758812354607215, 4.665393561625732488, -232.5634757513959983 ) ) ;
#1532 = CARTESIAN_POINT ( 'NONE',  ( 5.964915545484365644, 11.50358694729900577, -229.9646467236423462 ) ) ;
#1533 = CARTESIAN_POINT ( 'NONE',  ( 21.28562020585086501, -15.94148943779260819, -218.1725164024425396 ) ) ;
#1534 = DIRECTION ( 'NONE',  ( -0.000000000000000000, -0.000000000000000000, -1.000000000000000000 ) ) ;
#1535 = ORIENTED_EDGE ( 'NONE', *, *, #21161, .T. ) ;
#1536 = CARTESIAN_POINT ( 'NONE',  ( -15.20262116893801974, 8.038155052917188570, -217.6767387945475036 ) ) ;
#1537 = CARTESIAN_POINT ( 'NONE',  ( -17.92393051735373888, -14.45097846726422830, -234.9711082062119374 ) ) ;
#1538 = CARTESIAN_POINT ( 'NONE',  ( 0.000000000000000000, 0.000000000000000000, -120.0000000000000142 ) ) ;
#1539 = CARTESIAN_POINT ( 'NONE',  ( 5.069241901512100412, 14.34986542013820632, -229.6420000777802954 ) ) ;
#1540 = CARTESIAN_POINT ( 'NONE',  ( 0.000000000000000000, 0.000000000000000000, -75.00000000000000000 ) ) ;
#1541 = CARTESIAN_POINT ( 'NONE',  ( 11.90144651507291051, -8.898305237537579515, -228.5592478859710184 ) ) ;
#1542 = CARTESIAN_POINT ( 'NONE',  ( -25.29098058636142810, 5.014641116111857144, -217.4658967307323110 ) ) ;
#1543 = CIRCLE ( 'NONE', #9800, 25.00000000000000000 ) ;
#1544 = AXIS2_PLACEMENT_3D ( 'NONE', #2541, #8986, #15960 ) ;
#1545 = CARTESIAN_POINT ( 'NONE',  ( 21.14328650935969023, 6.072767611243683916, -217.6422864096696514 ) ) ;
#1546 = SHAPE_REPRESENTATION ( 'Frothing Whisk', ( #6677 ), #13476 ) ;
#1547 = CARTESIAN_POINT ( 'NONE',  ( -5.534391910549205207, -14.54353160188980709, -228.1022699408985943 ) ) ;
#1548 = CIRCLE ( 'NONE', #4759, 21.63401512838748175 ) ;
#1549 = PLANE ( 'NONE',  #9838 ) ;
#1550 = CARTESIAN_POINT ( 'NONE',  ( 18.54610009393809023, 0.6523581019769808531, -231.1787333216317677 ) ) ;
#1551 = CARTESIAN_POINT ( 'NONE',  ( 0.000000000000000000, 0.000000000000000000, -55.00000000000000000 ) ) ;
#1552 = CARTESIAN_POINT ( 'NONE',  ( 11.40994021191102092, -13.94644022156852969, -230.1289083636806936 ) ) ;
#1554 = ADVANCED_FACE ( 'NONE', ( #18239 ), #2363, .T. ) ;
#1553 = CARTESIAN_POINT ( 'NONE',  ( 12.99467735515414191, -2.323045947487815788, -223.0925300893006238 ) ) ;
#1555 = CARTESIAN_POINT ( 'NONE',  ( -20.71254002826594842, -9.999534281261636792, -0.6688830150170183009 ) ) ;
#1556 = CARTESIAN_POINT ( 'NONE',  ( 14.66646255503707152, 18.43809875292740230, -219.3480462970252063 ) ) ;
#1557 = CARTESIAN_POINT ( 'NONE',  ( 8.539351012053531420, 16.03230746435535181, -220.6282946404833751 ) ) ;
#1558 = CARTESIAN_POINT ( 'NONE',  ( 22.27668549480667792, -16.40903445915953895, -216.4638184065479152 ) ) ;
#1559 = CARTESIAN_POINT ( 'NONE',  ( 9.104026917753444081, -10.66572815660443041, -221.9193219976906448 ) ) ;
#1560 = EDGE_LOOP ( 'NONE', ( #10535, #10990, #6034, #13613, #17716, #18477 ) ) ;
#1561 = CARTESIAN_POINT ( 'NONE',  ( -8.435479365662203577, 14.12888021429238528, -220.5365774424437859 ) ) ;
#1562 = CARTESIAN_POINT ( 'NONE',  ( -17.55809605150417951, 6.636094600389130349, -229.8856864643722986 ) ) ;
#1563 = CARTESIAN_POINT ( 'NONE',  ( 21.15841376125116824, 4.865517895153391947, -217.1795922978051578 ) ) ;
#1564 = VERTEX_POINT ( 'NONE', #6072 ) ;
#1565 = CARTESIAN_POINT ( 'NONE',  ( -5.427686778165598191, -19.74436295060356272, -231.6150980610854901 ) ) ;
#1566 = CARTESIAN_POINT ( 'NONE',  ( 1.509788170712047295, -10.75822951548915007, 92.00000000000001421 ) ) ;
#1567 = AXIS2_PLACEMENT_3D ( 'NONE', #14727, #987, #14093 ) ;
#1568 = CARTESIAN_POINT ( 'NONE',  ( -11.89542918462869103, -0.2773029175206048191, -224.4556830488584467 ) ) ;
#1569 = ORIENTED_EDGE ( 'NONE', *, *, #7048, .T. ) ;
#1570 = AXIS2_PLACEMENT_3D ( 'NONE', #16970, #6954, #8425 ) ;
#1571 = CARTESIAN_POINT ( 'NONE',  ( 19.97628502126439187, 24.50819884991013708, -224.8824979922784735 ) ) ;
#1572 = CARTESIAN_POINT ( 'NONE',  ( 12.63976474005154493, -11.16289257830726278, -221.8494566150397134 ) ) ;
#1573 = EDGE_CURVE ( 'NONE', #2436, #16180, #2800, .T. ) ;
#1574 = CARTESIAN_POINT ( 'NONE',  ( 9.107417252317809186, 16.30291009569977234, -218.0131178633739921 ) ) ;
#1575 = CARTESIAN_POINT ( 'NONE',  ( -16.71711190488355570, 0.6105529133557690002, -230.9511258789794681 ) ) ;
#1576 = CARTESIAN_POINT ( 'NONE',  ( 11.50837930502119733, 10.86662242793286381, -233.1728506169798436 ) ) ;
#1577 = CARTESIAN_POINT ( 'NONE',  ( -22.14646582578067679, 6.967411055428133437, -231.6932229095398270 ) ) ;
#1578 = CARTESIAN_POINT ( 'NONE',  ( -11.26857159993117996, 28.96895336474501192, -225.6039696848669678 ) ) ;
#1579 = DIRECTION ( 'NONE',  ( 0.03647168421188083653, 0.3315607655626302552, 0.9427286327412950362 ) ) ;
#1580 = CARTESIAN_POINT ( 'NONE',  ( 5.609436632608550966, -13.11664087352601094, -229.3324225951633650 ) ) ;
#1581 = CARTESIAN_POINT ( 'NONE',  ( 14.62702828724412285, -1.994068170757606673, -224.0552340365271959 ) ) ;
#1582 = CARTESIAN_POINT ( 'NONE',  ( 0.000000000000000000, 0.000000000000000000, 69.99999999999998579 ) ) ;
#1583 = CARTESIAN_POINT ( 'NONE',  ( -15.89118508636071958, -1.798691612803976492, -229.3605869667087234 ) ) ;
#1584 = CARTESIAN_POINT ( 'NONE',  ( 16.64225601860865211, 1.926018578292457928, -220.2177910260893725 ) ) ;
#1585 = CARTESIAN_POINT ( 'NONE',  ( -10.37556110177195023, -11.10057404503678846, -224.0577835142470349 ) ) ;
#1586 = CARTESIAN_POINT ( 'NONE',  ( 16.02266676603872142, -2.327704065170765110E-15, -100.7764571353075524 ) ) ;
#1587 = SURFACE_STYLE_FILL_AREA ( #3257 ) ;
#1588 = CARTESIAN_POINT ( 'NONE',  ( 11.64632602964496044, -20.35392056169815689, -232.5450580586399383 ) ) ;
#1589 = CARTESIAN_POINT ( 'NONE',  ( -18.14952719657095415, 1.368063294522122275, -218.0005379682515922 ) ) ;
#1590 = CARTESIAN_POINT ( 'NONE',  ( -8.611121136347097860, 17.46802294375265419, -231.5575697815534113 ) ) ;
#1591 = CARTESIAN_POINT ( 'NONE',  ( -7.626320092023432196, 21.25423560278784407, -233.8867968595558295 ) ) ;
#1592 = CARTESIAN_POINT ( 'NONE',  ( 12.55122320111375700, -1.519965464208375749, -221.0350040576933281 ) ) ;
#1593 = CARTESIAN_POINT ( 'NONE',  ( 12.04687593227112430, 27.54339840196571743, -224.6466266724203820 ) ) ;
#1594 = CARTESIAN_POINT ( 'NONE',  ( -24.19163806436329978, 8.131440952769249719, -230.9341214615949127 ) ) ;
#1595 = CARTESIAN_POINT ( 'NONE',  ( 17.98589043827631428, 2.945998030785370592, -233.4030907785035538 ) ) ;
#1596 = EDGE_CURVE ( 'NONE', #16287, #758, #10152, .T. ) ;
#1597 = DIRECTION ( 'NONE',  ( 1.000000000000000000, 0.000000000000000000, 0.000000000000000000 ) ) ;
#1598 = CARTESIAN_POINT ( 'NONE',  ( 9.774133712851615030, 11.09751083462123766, -229.6876724410067823 ) ) ;
#1599 = AXIS2_PLACEMENT_3D ( 'NONE', #21798, #1216, #5136 ) ;
#1600 = CARTESIAN_POINT ( 'NONE',  ( -18.90911063232017142, 5.352531560950812839, -219.6301177803536575 ) ) ;
#1601 = CARTESIAN_POINT ( 'NONE',  ( 2.631948090663005946, 31.21493676147814611, -222.3107766067421380 ) ) ;
#1602 = CARTESIAN_POINT ( 'NONE',  ( 11.75630001506626776, 9.075791953625659048, -230.4239556728226717 ) ) ;
#1603 = CARTESIAN_POINT ( 'NONE',  ( -13.04380155829002419, -28.08004287256819609, -224.7912146079995352 ) ) ;
#1604 = VERTEX_POINT ( 'NONE', #785 ) ;
#1605 = CARTESIAN_POINT ( 'NONE',  ( -5.218961787268129093, -16.18493974670746027, -219.8229902141834771 ) ) ;
#1606 = CARTESIAN_POINT ( 'NONE',  ( -12.19796877179171446, 17.24929682309303658, -234.5722138766719809 ) ) ;
#1607 = CARTESIAN_POINT ( 'NONE',  ( 2.098184199980985376, -13.29281380427311099, -222.1652846463370281 ) ) ;
#1608 = CARTESIAN_POINT ( 'NONE',  ( -2.808235066048971440, 30.42019778760651150, -222.6481917607299295 ) ) ;
#1609 = CARTESIAN_POINT ( 'NONE',  ( 13.04627209130898002, -4.074791396861574988, -220.3858784301183675 ) ) ;
#1610 = CARTESIAN_POINT ( 'NONE',  ( -24.92024473536680773, -13.74570206812420103, -220.1598944320903115 ) ) ;
#1611 = CARTESIAN_POINT ( 'NONE',  ( 12.63974878616558328, 15.03448928898568759, -231.7036488814491406 ) ) ;
#1612 = CARTESIAN_POINT ( 'NONE',  ( 0.000000000000000000, 23.00000000000000000, 75.00000000000000000 ) ) ;
#1613 = CARTESIAN_POINT ( 'NONE',  ( -27.17783334270200157, 15.20409188923851751, -223.6555185980277258 ) ) ;
#1614 = CARTESIAN_POINT ( 'NONE',  ( 16.43556216695724004, 8.397919695511960825, -216.7971521583719152 ) ) ;
#1615 = AXIS2_PLACEMENT_3D ( 'NONE', #17502, #2069, #8949 ) ;
#1616 = CARTESIAN_POINT ( 'NONE',  ( 22.02796522526679723, 16.41909032291435366, -220.1590600991317217 ) ) ;
#1617 = CARTESIAN_POINT ( 'NONE',  ( 15.56183105618911355, 23.93598532278018354, -223.2746693648072664 ) ) ;
#1618 = CARTESIAN_POINT ( 'NONE',  ( 4.956111054478943068, -16.91316901532391270, -234.1076498343193748 ) ) ;
#1619 = CARTESIAN_POINT ( 'NONE',  ( -11.10144104376680652, 18.49675466419975578, -232.2931259015917647 ) ) ;
#1620 = ADVANCED_FACE ( 'NONE', ( #14536 ), #3699, .F. ) ;
#1621 = CARTESIAN_POINT ( 'NONE',  ( 19.20300624114736721, 0.6066039755357417462, -231.5046416827383950 ) ) ;
#1622 = CARTESIAN_POINT ( 'NONE',  ( 7.717439423011566824, -15.08909893080012132, -230.2794769249191518 ) ) ;
#1623 = CARTESIAN_POINT ( 'NONE',  ( -13.70798801564395752, 13.71024986321384809, -218.3360451569033955 ) ) ;
#1624 = CARTESIAN_POINT ( 'NONE',  ( -2.435715273212520238, 23.41098772907853132, -217.6796576669356966 ) ) ;
#1625 = CARTESIAN_POINT ( 'NONE',  ( -25.82802808205240552, -14.78441951539553401, -222.6940535085979604 ) ) ;
#1626 = CARTESIAN_POINT ( 'NONE',  ( 18.40125535140034430, 0.01434342441762339639, -233.2485400239426099 ) ) ;
#1628 = CARTESIAN_POINT ( 'NONE',  ( 11.00045714400293306, 20.20239058357963913, -215.1666500215986275 ) ) ;
#1627 = AXIS2_PLACEMENT_3D ( 'NONE', #997, #7872, #9772 ) ;
#1629 = EDGE_LOOP ( 'NONE', ( #4957, #10753, #10472, #18603 ) ) ;
#1630 = CARTESIAN_POINT ( 'NONE',  ( 12.10245006109274080, 26.02147364279441888, -220.6079829738538649 ) ) ;
#1631 = CARTESIAN_POINT ( 'NONE',  ( 23.53402537799887284, -10.66620622184993650, -219.3119847637072439 ) ) ;
#1632 = AXIS2_PLACEMENT_3D ( 'NONE', #2945, #9501, #9832 ) ;
#1633 = CARTESIAN_POINT ( 'NONE',  ( 22.55746627616819566, -14.21542447219996852, -231.9819121152456205 ) ) ;
#1634 =( LENGTH_UNIT ( ) NAMED_UNIT ( * ) SI_UNIT ( .MILLI., .METRE. ) );
#1635 = CARTESIAN_POINT ( 'NONE',  ( 0.7245137624042983227, 13.44764381486384330, -223.4043886706536455 ) ) ;
#1636 = CARTESIAN_POINT ( 'NONE',  ( -10.91546170668013005, -7.896971223757457636, -230.5866998909293102 ) ) ;
#1637 = CARTESIAN_POINT ( 'NONE',  ( -10.11868820210310282, -13.51996935893276053, -218.1704188629865371 ) ) ;
#1638 = CARTESIAN_POINT ( 'NONE',  ( 6.741123954526870854, -14.00899218320067341, -219.0418835583997179 ) ) ;
#1639 = CARTESIAN_POINT ( 'NONE',  ( -8.791002657293931932, 17.82034842365333205, -218.5247019341474584 ) ) ;
#1640 = CARTESIAN_POINT ( 'NONE',  ( 8.250760074138732136, 14.96691001493985951, -221.7548416114337613 ) ) ;
#1641 = CARTESIAN_POINT ( 'NONE',  ( -17.79285498209129202, 9.187865686019035749, -216.3798185811636756 ) ) ;
#1642 = CARTESIAN_POINT ( 'NONE',  ( -31.12406087576577463, 7.316399946619934092, -225.0171288978685027 ) ) ;
#1643 = CARTESIAN_POINT ( 'NONE',  ( -15.15256618962804858, -12.22297499669621423, -230.3735341043967821 ) ) ;
#1644 = VERTEX_POINT ( 'NONE', #11142 ) ;
#1645 = CARTESIAN_POINT ( 'NONE',  ( -4.784012432433236484, 23.31984772163034947, -232.0554186943449508 ) ) ;
#1646 = EDGE_CURVE ( 'NONE', #19741, #19867, #11223, .T. ) ;
#1647 = CARTESIAN_POINT ( 'NONE',  ( 14.33191776452776622, 5.147404080619256916, -219.0172570056664938 ) ) ;
#1648 = CARTESIAN_POINT ( 'NONE',  ( 24.61409543538958289, 19.88121288930873476, -228.5015986536257344 ) ) ;
#1649 = CARTESIAN_POINT ( 'NONE',  ( 12.90474009670415967, -3.145873754258878385, -224.5449843457338375 ) ) ;
#1650 = DIRECTION ( 'NONE',  ( 0.000000000000000000, 0.000000000000000000, -1.000000000000000000 ) ) ;
#1651 = ORIENTED_EDGE ( 'NONE', *, *, #15761, .F. ) ;
#1652 =( GEOMETRIC_REPRESENTATION_CONTEXT ( 3 ) GLOBAL_UNCERTAINTY_ASSIGNED_CONTEXT ( ( #16412 ) ) GLOBAL_UNIT_ASSIGNED_CONTEXT ( ( #9478, #6196, #11385 ) ) REPRESENTATION_CONTEXT ( 'NONE', 'WORKASPACE' ) );
#1653 = CARTESIAN_POINT ( 'NONE',  ( -7.429838964355703901, 14.87322129099639234, -232.2632863647814077 ) ) ;
#1654 = CARTESIAN_POINT ( 'NONE',  ( -23.48355816166749932, -5.921172941748132246, -214.8630305010649408 ) ) ;
#1655 = DIRECTION ( 'NONE',  ( -1.000000000000000000, 0.000000000000000000, 0.000000000000000000 ) ) ;
#1656 = CARTESIAN_POINT ( 'NONE',  ( 25.33562512631297281, 12.25422971834577268, -228.6777356031426791 ) ) ;
#1657 = CARTESIAN_POINT ( 'NONE',  ( -20.26851768784797869, -0.8260594303982465858, -217.1279713726092098 ) ) ;
#1658 = CARTESIAN_POINT ( 'NONE',  ( 10.24538335401965661, -11.82980241027587276, -219.3753974371782363 ) ) ;
#1659 = CARTESIAN_POINT ( 'NONE',  ( -18.08305592660031991, 4.022743421239192152, -217.2335041149100050 ) ) ;
#1660 = CARTESIAN_POINT ( 'NONE',  ( 14.68015846516680867, 2.651775288685355836, -224.1317433549420173 ) ) ;
#1661 = CARTESIAN_POINT ( 'NONE',  ( -6.454554286546707154, -27.99704349260872149, -227.4356265632874852 ) ) ;
#1662 = LINE ( 'NONE', #17085, #13418 ) ;
#1663 = CARTESIAN_POINT ( 'NONE',  ( 24.03642272140365677, 3.646960756862087205, -218.2320643939070806 ) ) ;
#1664 = CARTESIAN_POINT ( 'NONE',  ( 0.000000000000000000, 23.00000000000006040, 75.00000000000000000 ) ) ;
#1665 = CARTESIAN_POINT ( 'NONE',  ( 14.47405021949252557, -20.16114635186222159, -231.2055612633458566 ) ) ;
#1666 = TOROIDAL_SURFACE ( 'NONE', #17127, 24.63401512838748530, 3.000000000000004441 ) ;
#1667 = DIRECTION ( 'NONE',  ( -2.162300680179986877E-16, -1.000000000000000000, 0.000000000000000000 ) ) ;
#1668 = CARTESIAN_POINT ( 'NONE',  ( -21.01325146862401638, -9.352110752727961440, -3.555790053721613830 ) ) ;
#1669 = CARTESIAN_POINT ( 'NONE',  ( 9.280831573919673616, 14.67893982993557422, -228.6940810986570796 ) ) ;
#1670 = CARTESIAN_POINT ( 'NONE',  ( 8.312165662451315384, 13.84431584962456974, -225.8109542921768025 ) ) ;
#1671 = CARTESIAN_POINT ( 'NONE',  ( 20.62543286083822380, -24.26207512693059343, -224.4080524747341201 ) ) ;
#1672 = CARTESIAN_POINT ( 'NONE',  ( 15.34510829589250491, -24.56813251781886009, -230.1307231235174982 ) ) ;
#1673 = ORIENTED_EDGE ( 'NONE', *, *, #20807, .T. ) ;
#1674 = ADVANCED_FACE ( 'NONE', ( #1114 ), #14825, .T. ) ;
#1675 = CARTESIAN_POINT ( 'NONE',  ( -22.07068341299880743, 18.38202870573248049, -227.7785760498121306 ) ) ;
#1676 = CARTESIAN_POINT ( 'NONE',  ( -17.99155049254074612, 5.190958499132906745, -220.1449419322306937 ) ) ;
#1677 = CARTESIAN_POINT ( 'NONE',  ( 15.70179827786738969, 6.572001003133339125, -229.5476218741844434 ) ) ;
#1678 = ORIENTED_EDGE ( 'NONE', *, *, #12038, .T. ) ;
#1679 = CARTESIAN_POINT ( 'NONE',  ( -14.02781974392415165, -24.18658813864446344, -225.1634145543362706 ) ) ;
#1680 = CARTESIAN_POINT ( 'NONE',  ( -7.838405800256100342, -7.387516090585425133, 92.00000000000000000 ) ) ;
#1681 = ORIENTED_EDGE ( 'NONE', *, *, #18966, .T. ) ;
#1682 = CARTESIAN_POINT ( 'NONE',  ( 15.18181359483165949, 6.369295616116027681, -230.7949408486033462 ) ) ;
#1683 = CARTESIAN_POINT ( 'NONE',  ( 15.70595326690115634, -18.65841243762358559, -219.6423885132037981 ) ) ;
#1684 = CARTESIAN_POINT ( 'NONE',  ( 15.12287735332712835, 21.03907941686458116, -231.7894952627153202 ) ) ;
#1685 = CARTESIAN_POINT ( 'NONE',  ( -6.282398543089500187, 12.01615879894893801, -228.5121145169883903 ) ) ;
#1686 = ADVANCED_FACE ( 'NONE', ( #14531, #18010 ), #13270, .T. ) ;
#1687 = CARTESIAN_POINT ( 'NONE',  ( 6.550054208186137039, 12.38618022562281595, -231.5087189857719068 ) ) ;
#1688 = CARTESIAN_POINT ( 'NONE',  ( -10.83439284573031536, 18.36737820296253432, -234.3014274143859836 ) ) ;
#1689 = CARTESIAN_POINT ( 'NONE',  ( -8.823862513872974489, 14.92351368520778898, -217.1499513473673346 ) ) ;
#1690 = DIRECTION ( 'NONE',  ( 1.000000000000000000, 0.000000000000000000, 0.000000000000000000 ) ) ;
#1691 = CARTESIAN_POINT ( 'NONE',  ( -3.300598509645395584, -18.18730530649546395, -233.4303386612170925 ) ) ;
#1692 = CARTESIAN_POINT ( 'NONE',  ( 1.387778780781445676E-13, -19.79999999999999716, -78.50000000000000000 ) ) ;
#1693 = DIRECTION ( 'NONE',  ( -1.000000000000000000, -0.000000000000000000, -0.000000000000000000 ) ) ;
#1694 = PRODUCT_DEFINITION_SHAPE ( 'NONE', 'NONE',  #7130 ) ;
#1695 = CARTESIAN_POINT ( 'NONE',  ( -29.27492217116574480, -1.185422171198730501, -224.8132346143397342 ) ) ;
#1696 = CARTESIAN_POINT ( 'NONE',  ( 22.18132842682159733, 5.591149267797686839, -232.0584733989884114 ) ) ;
#1697 = CARTESIAN_POINT ( 'NONE',  ( -14.57915343259292307, -9.548365625374035659, -229.2620333697842057 ) ) ;
#1698 = CARTESIAN_POINT ( 'NONE',  ( 9.759123193367146953, -21.89695672029116480, -217.8292787338521919 ) ) ;
#1699 = CARTESIAN_POINT ( 'NONE',  ( -21.43408368508570305, 3.680162304907783621, -233.1134812316964542 ) ) ;
#1700 = CARTESIAN_POINT ( 'NONE',  ( -0.9249541874382023465, 14.55235618511626328, -223.7321818898853962 ) ) ;
#1701 = CARTESIAN_POINT ( 'NONE',  ( -6.702936938788568888, 25.88675107068059944, -218.1129661040884287 ) ) ;
#1702 = CARTESIAN_POINT ( 'NONE',  ( 11.91821674756695693, -1.593691010653677242, -227.2895864140137405 ) ) ;
#1703 = EDGE_LOOP ( 'NONE', ( #10346, #17287, #5811, #6098 ) ) ;
#1704 = CARTESIAN_POINT ( 'NONE',  ( 14.39473142419577023, 15.98257177912839389, -217.4557725731239373 ) ) ;
#1705 = CARTESIAN_POINT ( 'NONE',  ( -19.27153818831731158, 23.75761453444584248, -221.9111479746408975 ) ) ;
#1706 = CARTESIAN_POINT ( 'NONE',  ( -11.59479561055411345, 9.544396733298208702, -229.1494558965577255 ) ) ;
#1707 = CARTESIAN_POINT ( 'NONE',  ( -10.39692419770002552, -10.11462123336039021, -222.6538761800393047 ) ) ;
#1708 = DIRECTION ( 'NONE',  ( -0.000000000000000000, 0.000000000000000000, -1.000000000000000000 ) ) ;
#1709 = CARTESIAN_POINT ( 'NONE',  ( 12.81769551943392393, 4.437328497131001193, -221.7762769673541072 ) ) ;
#1710 = CARTESIAN_POINT ( 'NONE',  ( -20.41147829968989313, 3.432784889297933795, -230.9611049257633510 ) ) ;
#1711 = CARTESIAN_POINT ( 'NONE',  ( 13.12946830070648652, 6.370976456471619365, -231.5124810213676483 ) ) ;
#1712 = CARTESIAN_POINT ( 'NONE',  ( 15.28706223449149348, 2.473424253736659306, -227.9634568993954531 ) ) ;
#1713 = CARTESIAN_POINT ( 'NONE',  ( -9.698809215651296611, -24.51491891025427350, -232.5150754403024962 ) ) ;
#1714 = ORIENTED_EDGE ( 'NONE', *, *, #18092, .T. ) ;
#1715 = CARTESIAN_POINT ( 'NONE',  ( -10.94940667656068634, -10.80050631132953498, -220.7362776234490127 ) ) ;
#1716 = EDGE_CURVE ( 'NONE', #10973, #3502, #2231, .T. ) ;
#1717 = CARTESIAN_POINT ( 'NONE',  ( -18.07648963816576781, 14.36622924931724654, -235.1425738388569187 ) ) ;
#1718 = CARTESIAN_POINT ( 'NONE',  ( 11.32394539683753720, -15.63383003174572572, -233.0723040138117881 ) ) ;
#1719 = CARTESIAN_POINT ( 'NONE',  ( -10.45786516112131892, 23.61456281964591852, -233.2869923610001592 ) ) ;
#1720 = CARTESIAN_POINT ( 'NONE',  ( 29.08354724566992644, -8.084875104304042992, -220.4391609833976133 ) ) ;
#1721 = CARTESIAN_POINT ( 'NONE',  ( -16.64477864544768337, -2.947896226079009807, -219.6737919733007516 ) ) ;
#1722 = EDGE_CURVE ( 'NONE', #12201, #9941, #15183, .T. ) ;
#1723 = CARTESIAN_POINT ( 'NONE',  ( 26.75666476377482539, 8.100664119735744961, -232.1611550320539834 ) ) ;
#1724 = CARTESIAN_POINT ( 'NONE',  ( -17.50000000000000711, 0.000000000000000000, -55.00000000000000000 ) ) ;
#1725 = CARTESIAN_POINT ( 'NONE',  ( -6.573387563318148885, 17.69612765735440973, -231.1211991061559274 ) ) ;
#1726 = CARTESIAN_POINT ( 'NONE',  ( 12.43753614017300713, 2.441361880258234862, -222.2750447601761721 ) ) ;
#1727 = CARTESIAN_POINT ( 'NONE',  ( 10.78187269046063435, 10.73871010366167944, -221.9206544238666368 ) ) ;
#1728 = CARTESIAN_POINT ( 'NONE',  ( 28.53243699394185384, 6.329221954355706004, -218.6437889135959267 ) ) ;
#1729 = CARTESIAN_POINT ( 'NONE',  ( -3.300732473188277005, -24.68991359470437175, -216.3853901891898488 ) ) ;
#1730 = CARTESIAN_POINT ( 'NONE',  ( 2.291262277241625345, 17.20278591336981222, -216.2185160402476924 ) ) ;
#1731 = DIRECTION ( 'NONE',  ( -1.000000000000000000, -1.224646799147353454E-16, 0.000000000000000000 ) ) ;
#1732 = CARTESIAN_POINT ( 'NONE',  ( 2.478093603766003294, -30.50979708220057063, -227.6059245187310012 ) ) ;
#1733 = CARTESIAN_POINT ( 'NONE',  ( -24.79507334250576278, 6.844873424762779379, -218.1074956078844878 ) ) ;
#1734 = CARTESIAN_POINT ( 'NONE',  ( -2.692720963948733282, 24.67937284847025481, -218.0912907784291406 ) ) ;
#1735 = CARTESIAN_POINT ( 'NONE',  ( -12.13177435108894642, -8.392035797555511323, -228.8392847287196332 ) ) ;
#1736 = CARTESIAN_POINT ( 'NONE',  ( 26.91963614581376874, 6.107751173605064920, -232.2246916053503298 ) ) ;
#1737 = AXIS2_PLACEMENT_3D ( 'NONE', #10092, #15720, #17402 ) ;
#1738 = CARTESIAN_POINT ( 'NONE',  ( 18.69149182921226782, 24.00661454656289706, -229.8257469855424517 ) ) ;
#1739 = CARTESIAN_POINT ( 'NONE',  ( 7.168644370073567806, 19.32044210858112265, -233.1278450877711634 ) ) ;
#1740 = CARTESIAN_POINT ( 'NONE',  ( 13.95302107590712737, -11.87212821339389812, -220.3052895324516385 ) ) ;
#1741 = CARTESIAN_POINT ( 'NONE',  ( 10.05733608402134216, -9.620616164199983444, -224.9449885650552119 ) ) ;
#1742 = DIRECTION ( 'NONE',  ( 0.000000000000000000, 0.000000000000000000, 1.000000000000000000 ) ) ;
#1743 = CARTESIAN_POINT ( 'NONE',  ( 11.57669841200422134, 10.63052136557218574, -228.9489978335593889 ) ) ;
#1744 = CARTESIAN_POINT ( 'NONE',  ( -13.68978490692228256, -5.239663260684684687, -218.7416303080107411 ) ) ;
#1745 = CARTESIAN_POINT ( 'NONE',  ( -15.62091161899253855, -26.00636881980398840, -222.1463585103649905 ) ) ;
#1746 = CARTESIAN_POINT ( 'NONE',  ( 12.02378739738799140, -16.98783239109716092, -233.4545636224233931 ) ) ;
#1747 = CARTESIAN_POINT ( 'NONE',  ( -13.44241955326339166, 15.88952131657459965, -217.2587743382015901 ) ) ;
#1748 = CARTESIAN_POINT ( 'NONE',  ( 19.59567110982616001, 18.11097967140601028, -228.7314497914969706 ) ) ;
#1749 = CARTESIAN_POINT ( 'NONE',  ( -14.83974801774860630, 13.71714848582103485, -216.0935642439352762 ) ) ;
#1750 = CARTESIAN_POINT ( 'NONE',  ( -15.57505478537380306, 24.84242291948262249, -225.5907943047649837 ) ) ;
#1751 = CARTESIAN_POINT ( 'NONE',  ( 20.33239098169031323, -9.013719117183370599, -216.4483480702011775 ) ) ;
#1752 = CARTESIAN_POINT ( 'NONE',  ( -4.142636420702924482, 14.17169704882741321, -225.1666440184957310 ) ) ;
#1753 = CARTESIAN_POINT ( 'NONE',  ( 26.91963614581376874, 6.107751173605064920, -232.2246916053503298 ) ) ;
#1754 = CARTESIAN_POINT ( 'NONE',  ( 14.75291830987536557, 13.43762972591284033, -235.1407057970265839 ) ) ;
#1755 = CIRCLE ( 'NONE', #9316, 22.56777165119825668 ) ;
#1756 = CARTESIAN_POINT ( 'NONE',  ( 16.18295504345472580, -4.390854861972272261, -232.0514848646187716 ) ) ;
#1757 = DIRECTION ( 'NONE',  ( -1.000000000000000000, 0.000000000000000000, 0.000000000000000000 ) ) ;
#1758 = ORIENTED_EDGE ( 'NONE', *, *, #16835, .F. ) ;
#1759 = CARTESIAN_POINT ( 'NONE',  ( 0.6364901924797052857, 13.89978473517355617, -221.8840706290426397 ) ) ;
#1760 = CARTESIAN_POINT ( 'NONE',  ( -11.66037817688884992, -1.871521667041048609, -223.1840616512448037 ) ) ;
#1761 = LINE ( 'NONE', #8635, #13730 ) ;
#1762 = CARTESIAN_POINT ( 'NONE',  ( 13.49011766416699842, 7.659170998773840111, -228.1905628957712793 ) ) ;
#1763 = CARTESIAN_POINT ( 'NONE',  ( -13.10651848559790444, 3.262242204071156948, -224.3513854875720597 ) ) ;
#1764 = CARTESIAN_POINT ( 'NONE',  ( 11.78320976064766690, -8.193118641535518165, -222.2581747538435479 ) ) ;
#1765 = CARTESIAN_POINT ( 'NONE',  ( -18.46722752239034193, 0.9784074152395518809, -232.1633353206286188 ) ) ;
#1766 = CARTESIAN_POINT ( 'NONE',  ( -22.11084984981285118, 10.96048252433489623, -216.6117774006995376 ) ) ;
#1767 = CARTESIAN_POINT ( 'NONE',  ( 0.4703770282364683197, -28.19050476347214484, -228.5103440588500519 ) ) ;
#1768 = CARTESIAN_POINT ( 'NONE',  ( 1.317067778529001989E-13, -19.63401512838747820, 77.51594804401857175 ) ) ;
#1769 = CARTESIAN_POINT ( 'NONE',  ( -22.38013505867163389, 5.310942760180386024, 8.479298789953642057 ) ) ;
#1770 = CARTESIAN_POINT ( 'NONE',  ( -28.17543631911187063, 3.557555778861649642, -230.1980773687482156 ) ) ;
#1771 = CARTESIAN_POINT ( 'NONE',  ( 12.91525526572063853, -9.549346049255611035, -226.1928206613168584 ) ) ;
#1772 = CARTESIAN_POINT ( 'NONE',  ( 13.19509313252292060, -2.019678201665313644, -222.7800808301278437 ) ) ;
#1773 = CARTESIAN_POINT ( 'NONE',  ( -24.87078308609252630, 2.620408809423218077, 9.673169865297577275 ) ) ;
#1774 = CARTESIAN_POINT ( 'NONE',  ( 12.16813927252146144, 18.27141895336136912, -230.9123895730235745 ) ) ;
#1775 = CARTESIAN_POINT ( 'NONE',  ( 1.719513778997906694, 15.52930330544231730, -222.3959083836286368 ) ) ;
#1776 = CARTESIAN_POINT ( 'NONE',  ( -4.358491045216396742, -15.83376542237952300, -229.0450454480885583 ) ) ;
#1777 = CARTESIAN_POINT ( 'NONE',  ( 19.06435866915521515, -20.24829071055443563, -218.8318535520223804 ) ) ;
#1778 = CARTESIAN_POINT ( 'NONE',  ( -13.88743542672353826, 10.36310385030668613, -230.6144170796622745 ) ) ;
#1779 = CARTESIAN_POINT ( 'NONE',  ( -23.77327857871830830, 11.53128597905896768, -221.0855018166512025 ) ) ;
#1780 = CARTESIAN_POINT ( 'NONE',  ( -15.64716994811699813, 6.210654946517923491, -217.0002936794128345 ) ) ;
#1781 = CARTESIAN_POINT ( 'NONE',  ( -7.589660848220153078, -14.86992855705293692, -228.0480809167547136 ) ) ;
#1782 = CARTESIAN_POINT ( 'NONE',  ( -17.50000000000000355, 2.143131898507868643E-15, -25.00000000000000000 ) ) ;
#1783 = ORIENTED_EDGE ( 'NONE', *, *, #21371, .T. ) ;
#1784 = CARTESIAN_POINT ( 'NONE',  ( 15.33651282626308010, 7.807290788239344970, -218.6940806506825652 ) ) ;
#1785 = CARTESIAN_POINT ( 'NONE',  ( 13.59384321027942910, -22.95766697980085169, -228.5239052398278830 ) ) ;
#1786 = CARTESIAN_POINT ( 'NONE',  ( 17.19674704922021391, 23.07334190050143974, -228.8256488842130238 ) ) ;
#1787 = CARTESIAN_POINT ( 'NONE',  ( -7.913358619554302642, 16.16796202616373890, -233.0981776325470491 ) ) ;
#1788 = CARTESIAN_POINT ( 'NONE',  ( 14.17826651990317188, -1.167225063855702683, -222.4240311848849387 ) ) ;
#1789 = CARTESIAN_POINT ( 'NONE',  ( 0.7245137624042983227, 13.44764381486384330, -223.4043886706536455 ) ) ;
#1790 = CARTESIAN_POINT ( 'NONE',  ( 0.04718088033475073551, 10.76825293233556025, 91.99999999999998579 ) ) ;
#1791 = CARTESIAN_POINT ( 'NONE',  ( 1.729916699924999746, -18.64927252049523432, -233.5000329212076906 ) ) ;
#1792 = CARTESIAN_POINT ( 'NONE',  ( 13.96958060839473958, -9.488587112651741151, -218.7731372952745232 ) ) ;
#1793 = DIRECTION ( 'NONE',  ( -0.000000000000000000, 0.000000000000000000, -1.000000000000000000 ) ) ;
#1794 = CARTESIAN_POINT ( 'NONE',  ( -23.00000000000000000, 0.000000000000000000, -60.00000000000000000 ) ) ;
#1795 = CARTESIAN_POINT ( 'NONE',  ( -30.66857674073067130, 4.440060741118782239, -229.9901150862898476 ) ) ;
#1796 = CARTESIAN_POINT ( 'NONE',  ( -15.44264673875841432, -21.96030778071044054, -219.6531968376115174 ) ) ;
#1797 = CARTESIAN_POINT ( 'NONE',  ( 5.511302051500400090, -18.01881380728196902, -231.5522404100356084 ) ) ;
#1798 = CARTESIAN_POINT ( 'NONE',  ( 15.14859676485869500, 2.119979922547468032, -231.9009926880791284 ) ) ;
#1799 = CARTESIAN_POINT ( 'NONE',  ( 2.464084843620814702, 29.35663482419208492, -227.0015060686748143 ) ) ;
#1800 = CARTESIAN_POINT ( 'NONE',  ( -19.40752943788874774, 15.61499612050012864, -234.7624367253776541 ) ) ;
#1801 = EDGE_LOOP ( 'NONE', ( #4632, #13971, #7716, #8469 ) ) ;
#1802 = CARTESIAN_POINT ( 'NONE',  ( 30.72375212156453372, -9.269427080566114086, -227.3728682798597731 ) ) ;
#1803 = CARTESIAN_POINT ( 'NONE',  ( 21.35706335192880445, 15.67286272432725092, -219.2578158352350783 ) ) ;
#1804 = CARTESIAN_POINT ( 'NONE',  ( -24.53276002501160136, 17.12571705644413811, -226.2419685911331442 ) ) ;
#1805 = CARTESIAN_POINT ( 'NONE',  ( -24.33894786102607455, 16.69464852328507831, -227.6320542475859554 ) ) ;
#1806 = CARTESIAN_POINT ( 'NONE',  ( -14.26331330459994540, -11.99770975811722451, -232.1846756268951708 ) ) ;
#1807 = CARTESIAN_POINT ( 'NONE',  ( 0.000000000000000000, 17.50000000000000711, -24.99999999999999645 ) ) ;
#1808 = CARTESIAN_POINT ( 'NONE',  ( 14.33191776452776622, 5.147404080619256916, -219.0172570056664938 ) ) ;
#1809 = CARTESIAN_POINT ( 'NONE',  ( -17.65560862077320081, 21.92186454631220371, -221.3776075196718693 ) ) ;
#1810 = CARTESIAN_POINT ( 'NONE',  ( 19.07698357483942786, 25.86742807064150895, -222.6991278896559834 ) ) ;
#1811 = CARTESIAN_POINT ( 'NONE',  ( 13.89183999136464820, 6.553741795688899252, -220.8646181278399752 ) ) ;
#1812 = CARTESIAN_POINT ( 'NONE',  ( -18.30187879049682209, -3.992092017665997972, -215.1717549395094693 ) ) ;
#1813 = EDGE_LOOP ( 'NONE', ( #16398, #4768, #9072, #7529 ) ) ;
#1814 = CARTESIAN_POINT ( 'NONE',  ( -13.01444359484612079, -23.32256785062423887, -219.1545357706015693 ) ) ;
#1815 = CARTESIAN_POINT ( 'NONE',  ( -9.439286754415764591, 28.32957437491962338, -228.7842975624562598 ) ) ;
#1816 = CARTESIAN_POINT ( 'NONE',  ( 6.427665535191954937, -16.40046818492683656, -232.5919299485929912 ) ) ;
#1817 = CARTESIAN_POINT ( 'NONE',  ( 2.008896548638861024, 20.64812324442097591, -233.5818019448501843 ) ) ;
#1818 = CARTESIAN_POINT ( 'NONE',  ( 25.69249634387097814, -4.932549985819596472, -232.9896235759753438 ) ) ;
#1819 = DIRECTION ( 'NONE',  ( -0.9940043559354229119, 0.1093404791529896669, -4.060016141862974029E-14 ) ) ;
#1820 = ADVANCED_FACE ( 'NONE', ( #4264 ), #5099, .T. ) ;
#1821 = CARTESIAN_POINT ( 'NONE',  ( 19.55931020704464274, 3.833820734573247346, -215.4549349108404783 ) ) ;
#1822 = FILL_AREA_STYLE ('',( #18935 ) ) ;
#1823 = CARTESIAN_POINT ( 'NONE',  ( -6.564517230509238743, 23.65597541655194647, -219.1225629381441991 ) ) ;
#1824 = CARTESIAN_POINT ( 'NONE',  ( 13.06430160593375689, 2.561628050526134182, -220.6026188403641299 ) ) ;
#1825 = CARTESIAN_POINT ( 'NONE',  ( 8.812073984913094904, 13.12649198322903210, -229.9172071780580495 ) ) ;
#1826 = CARTESIAN_POINT ( 'NONE',  ( 30.47710800431509170, 7.409378661937554789, -223.2007768404241688 ) ) ;
#1827 = CARTESIAN_POINT ( 'NONE',  ( 5.002389762228888870, -13.81148461055073362, -218.0662212534467983 ) ) ;
#1828 = CARTESIAN_POINT ( 'NONE',  ( 1.867752180833619713, 31.25122076096762669, -227.4007918511463231 ) ) ;
#1829 = FACE_OUTER_BOUND ( 'NONE', #331, .T. ) ;
#1830 = CARTESIAN_POINT ( 'NONE',  ( -4.226568860449858356, -15.17239585821433678, -217.2407179915541349 ) ) ;
#1831 = CARTESIAN_POINT ( 'NONE',  ( -7.464187997994982560, 14.20693289415472016, -228.8865298551900764 ) ) ;
#1832 = EDGE_CURVE ( 'NONE', #18642, #10960, #2554, .T. ) ;
#1833 = CARTESIAN_POINT ( 'NONE',  ( 1.939863782649466017, 28.20584428268631783, -229.4487744520996273 ) ) ;
#1834 = CARTESIAN_POINT ( 'NONE',  ( -16.64477864544768337, -2.947896226079009807, -219.6737919733007516 ) ) ;
#1835 = CARTESIAN_POINT ( 'NONE',  ( -16.03353370602922467, 4.897644413504528060, -222.5335369890782999 ) ) ;
#1836 = CARTESIAN_POINT ( 'NONE',  ( -17.00265675087485917, 7.324244386240115645, -218.5600005870616656 ) ) ;
#1837 = CARTESIAN_POINT ( 'NONE',  ( 28.09488075336259527, 3.911739131332936381, -227.7543364642411632 ) ) ;
#1838 = VERTEX_POINT ( 'NONE', #18450 ) ;
#1839 = CARTESIAN_POINT ( 'NONE',  ( 8.689059922489732912, 15.18271246186214363, -218.7354841152034908 ) ) ;
#1840 = CARTESIAN_POINT ( 'NONE',  ( 26.90273745076186884, -10.52087603942467808, -226.9519702360728957 ) ) ;
#1841 = ORIENTED_EDGE ( 'NONE', *, *, #2125, .F. ) ;
#1842 = CARTESIAN_POINT ( 'NONE',  ( 26.86480837698434243, -8.606671353193281249, -231.2046318962545683 ) ) ;
#1843 = CARTESIAN_POINT ( 'NONE',  ( -0.7879796667336372851, 21.22375955577181372, -219.1554080315090118 ) ) ;
#1844 = ORIENTED_EDGE ( 'NONE', *, *, #22184, .T. ) ;
#1845 = LINE ( 'NONE', #7151, #18501 ) ;
#1846 = CARTESIAN_POINT ( 'NONE',  ( 12.85408565574548412, 7.821283853063205171, -223.1248833997948111 ) ) ;
#1847 = CARTESIAN_POINT ( 'NONE',  ( -9.864471611369220128, -7.448779108659549841, -221.8449511945744064 ) ) ;
#1848 = CARTESIAN_POINT ( 'NONE',  ( -4.670971249126254499, -22.80666086768999890, -234.0323572959307512 ) ) ;
#1849 = CARTESIAN_POINT ( 'NONE',  ( 8.818493748348606331, -10.89961555176610375, -227.9481955143288303 ) ) ;
#1850 = CARTESIAN_POINT ( 'NONE',  ( -6.208492967940078877, 16.71913201805454463, -230.4912298573936766 ) ) ;
#1851 = DIRECTION ( 'NONE',  ( 1.000000000000000000, 0.000000000000000000, 0.000000000000000000 ) ) ;
#1852 = CARTESIAN_POINT ( 'NONE',  ( 13.38540196930496862, 9.639609424068478205, -227.8779021328794840 ) ) ;
#1853 = CARTESIAN_POINT ( 'NONE',  ( -20.94800339253696109, 4.477632454355491731, -216.5423208360950298 ) ) ;
#1854 = CARTESIAN_POINT ( 'NONE',  ( -12.67136363292824086, 22.56975222910433843, -219.0840033572168011 ) ) ;
#1855 = CARTESIAN_POINT ( 'NONE',  ( 29.37495210618232022, -3.074218464324032229, -220.1817713028459025 ) ) ;
#1856 = CIRCLE ( 'NONE', #6174, 23.00000000000000000 ) ;
#1857 = CARTESIAN_POINT ( 'NONE',  ( -0.7041916573665241152, 14.60214745152014437, -226.3818583194645555 ) ) ;
#1858 = CARTESIAN_POINT ( 'NONE',  ( -16.98287383830707142, 1.584866439881522648, -221.5391863673846444 ) ) ;
#1859 = CARTESIAN_POINT ( 'NONE',  ( 23.07558131619435571, 16.33594519118144817, -217.0553921114837124 ) ) ;
#1860 = CARTESIAN_POINT ( 'NONE',  ( 4.804712767000853368, -14.77773536573586455, -228.5128529893618747 ) ) ;
#1861 = CARTESIAN_POINT ( 'NONE',  ( -22.05223281125454804, 0.4748437386657365367, -217.8785187290425256 ) ) ;
#1862 = EDGE_LOOP ( 'NONE', ( #17430, #6696, #13469, #7808 ) ) ;
#1863 = CARTESIAN_POINT ( 'NONE',  ( -7.825349071214003693, 24.14595706726266755, -216.5959661901539732 ) ) ;
#1864 = CARTESIAN_POINT ( 'NONE',  ( -10.99009178837907186, -10.32629327015668785, -231.8361825614163365 ) ) ;
#1865 = CARTESIAN_POINT ( 'NONE',  ( 0.000000000000000000, 0.000000000000000000, -55.00000000000000000 ) ) ;
#1866 = AXIS2_PLACEMENT_3D ( 'NONE', #21754, #7827, #7933 ) ;
#1867 = CARTESIAN_POINT ( 'NONE',  ( 14.98418162551161714, 4.450317369940187895, -227.9894155827521161 ) ) ;
#1868 = CARTESIAN_POINT ( 'NONE',  ( -22.47200958260654957, 4.697452857301940732, -216.5879371680706242 ) ) ;
#1869 = CARTESIAN_POINT ( 'NONE',  ( 8.649266908999912573, -10.50942778440553482, -226.4415026780416440 ) ) ;
#1870 = CARTESIAN_POINT ( 'NONE',  ( -7.825349071214003693, 24.14595706726266755, -216.5959661901539732 ) ) ;
#1871 = CARTESIAN_POINT ( 'NONE',  ( -17.96792326766206926, -0.6237852504629022299, -217.9759415197746932 ) ) ;
#1872 = CARTESIAN_POINT ( 'NONE',  ( -6.723652888800149441, -28.28510889945508211, -226.1741921951756638 ) ) ;
#1873 = CARTESIAN_POINT ( 'NONE',  ( -22.63401512838748175, 0.000000000000000000, 77.51594804401857175 ) ) ;
#1874 = CARTESIAN_POINT ( 'NONE',  ( -22.62276587825132168, 4.159918992556371542, 9.099611153187048274 ) ) ;
#1875 = CARTESIAN_POINT ( 'NONE',  ( -11.79584727357715934, 6.509288465425584036, -222.6080315736180921 ) ) ;
#1876 = CARTESIAN_POINT ( 'NONE',  ( 10.38773686668317531, -11.52324865342443516, -226.2052026729718932 ) ) ;
#1877 = CARTESIAN_POINT ( 'NONE',  ( -28.87859926594958537, -0.8320174534291842061, -222.6356913548140142 ) ) ;
#1878 = CIRCLE ( 'NONE', #14472, 3.000000000000002665 ) ;
#1879 = CARTESIAN_POINT ( 'NONE',  ( -25.00000000000000355, 0.3288899015253046731, 9.999999999999998224 ) ) ;
#1880 = CARTESIAN_POINT ( 'NONE',  ( 27.30736127486511577, 7.960716467858479639, -228.6121938484450595 ) ) ;
#1881 = CARTESIAN_POINT ( 'NONE',  ( -20.38637754046084183, 19.95723714148678241, -217.5201383746364172 ) ) ;
#1882 = CARTESIAN_POINT ( 'NONE',  ( 13.38540196930496862, 9.639609424068478205, -227.8779021328794840 ) ) ;
#1883 = CARTESIAN_POINT ( 'NONE',  ( -0.4481215836501183380, -14.49514564254841353, -225.8120917640279970 ) ) ;
#1884 = CARTESIAN_POINT ( 'NONE',  ( 19.25263663724807728, -8.631913731826720948, -234.6583132812941983 ) ) ;
#1885 = ORIENTED_EDGE ( 'NONE', *, *, #955, .T. ) ;
#1886 = CARTESIAN_POINT ( 'NONE',  ( 2.630208337444488453, 16.40323635460054774, -219.2570070657488088 ) ) ;
#1887 = CARTESIAN_POINT ( 'NONE',  ( -25.20870746202117729, 11.68425842440532136, -223.9066764530103342 ) ) ;
#1888 = CARTESIAN_POINT ( 'NONE',  ( -21.39667546302236900, 3.687493526428279100, -235.1435990565495047 ) ) ;
#1889 = ORIENTED_EDGE ( 'NONE', *, *, #5608, .T. ) ;
#1890 = CARTESIAN_POINT ( 'NONE',  ( -16.02814206296035593, -12.75525137407698040, -230.7643788161867633 ) ) ;
#1891 = DIRECTION ( 'NONE',  ( -0.000000000000000000, -0.000000000000000000, -1.000000000000000000 ) ) ;
#1892 = ORIENTED_EDGE ( 'NONE', *, *, #12725, .F. ) ;
#1893 = CARTESIAN_POINT ( 'NONE',  ( 16.31458447723494132, 2.619382102851042671, -229.5862799001085364 ) ) ;
#1894 = CARTESIAN_POINT ( 'NONE',  ( 15.15335612453267089, -12.60200553607942098, -219.4566848265094166 ) ) ;
#1895 = CARTESIAN_POINT ( 'NONE',  ( 5.331555957413248059, 27.50712867803999728, -219.0801070358024276 ) ) ;
#1896 = EDGE_CURVE ( 'NONE', #5175, #645, #5150, .T. ) ;
#1897 = CARTESIAN_POINT ( 'NONE',  ( -17.39699619235753048, 15.64332637722790054, -216.0406373264262641 ) ) ;
#1898 = AXIS2_PLACEMENT_3D ( 'NONE', #489, #17488, #19159 ) ;
#1899 = AXIS2_PLACEMENT_3D ( 'NONE', #17393, #8729, #17277 ) ;
#1900 = CARTESIAN_POINT ( 'NONE',  ( 15.51445714770079931, 9.275596138242290678, -215.8565574371285436 ) ) ;
#1901 = CARTESIAN_POINT ( 'NONE',  ( 4.907833106823921376, 13.98151846258800290, -229.0190609869640923 ) ) ;
#1902 = CARTESIAN_POINT ( 'NONE',  ( 15.16859210357277554, 1.744254869442751099, -222.5574993570340609 ) ) ;
#1903 = CARTESIAN_POINT ( 'NONE',  ( -7.800954605602409053, -29.95157606033723496, -226.5906573908930000 ) ) ;
#1904 = CARTESIAN_POINT ( 'NONE',  ( 17.15627899979664051, -18.64955541608202694, -217.1729447097152388 ) ) ;
#1905 = DIRECTION ( 'NONE',  ( -1.000000000000000000, -6.982962677686266711E-15, 0.000000000000000000 ) ) ;
#1906 = CARTESIAN_POINT ( 'NONE',  ( 0.000000000000000000, 0.000000000000000000, -77.51594804401857175 ) ) ;
#1907 = CARTESIAN_POINT ( 'NONE',  ( -26.42613204384124259, 13.88327151024443395, -218.2510073314678323 ) ) ;
#1908 = CARTESIAN_POINT ( 'NONE',  ( -27.21693968233852701, -2.213369147249347524, -221.9579181326467392 ) ) ;
#1909 = AXIS2_PLACEMENT_3D ( 'NONE', #13871, #3496, #20254 ) ;
#1910 = AXIS2_PLACEMENT_3D ( 'NONE', #9554, #18324, #18550 ) ;
#1911 = CARTESIAN_POINT ( 'NONE',  ( 12.43753614017300713, 2.441361880258234862, -222.2750447601761721 ) ) ;
#1912 = CARTESIAN_POINT ( 'NONE',  ( -3.223980134944351317, 26.83284996841001302, -219.5167893230652965 ) ) ;
#1913 = CARTESIAN_POINT ( 'NONE',  ( 4.936777854427027989, 27.97379167488809060, -227.0886654730259124 ) ) ;
#1914 = ORIENTED_EDGE ( 'NONE', *, *, #4731, .F. ) ;
#1915 = CARTESIAN_POINT ( 'NONE',  ( 30.30544834784952002, -1.486206387887903047, -219.3838232483325896 ) ) ;
#1916 = VERTEX_POINT ( 'NONE', #20680 ) ;
#1917 = CARTESIAN_POINT ( 'NONE',  ( 15.61962121506769385, 4.525360868525488911, -229.0684696061408090 ) ) ;
#1918 = CARTESIAN_POINT ( 'NONE',  ( -13.01696012539752445, 9.878799299062107409, -218.8446158128127195 ) ) ;
#1919 = CARTESIAN_POINT ( 'NONE',  ( -15.23792247720107440, 7.806131751461257373, -230.3336101049160902 ) ) ;
#1920 = CARTESIAN_POINT ( 'NONE',  ( -19.02606456345395358, -20.49905271945607055, -219.9673098173381902 ) ) ;
#1921 = CARTESIAN_POINT ( 'NONE',  ( -26.02440924314744919, 2.824604386891162111, -232.0644005296583430 ) ) ;
#1922 = CARTESIAN_POINT ( 'NONE',  ( -22.97235139684061878, 2.813301660702908866E-15, 75.01817430661621700 ) ) ;
#1923 = CARTESIAN_POINT ( 'NONE',  ( -3.000000000000034195, 6.000000000000006217, -227.9999999999999716 ) ) ;
#1924 = CARTESIAN_POINT ( 'NONE',  ( 27.13894094332088969, 12.30518789341946295, -220.2765066586875093 ) ) ;
#1925 = AXIS2_PLACEMENT_3D ( 'NONE', #13735, #11707, #10354 ) ;
#1926 = CARTESIAN_POINT ( 'NONE',  ( -19.72392517715239535, 13.50888179936880107, -230.7714862421596251 ) ) ;
#1927 = CARTESIAN_POINT ( 'NONE',  ( 8.126072675580726212, 14.68573014611672534, -233.8823376361746966 ) ) ;
#1928 = CARTESIAN_POINT ( 'NONE',  ( 19.30248206944178335, -1.297331563427565726, -230.8957665284791290 ) ) ;
#1929 = CARTESIAN_POINT ( 'NONE',  ( -12.51550321509044927, -6.200974036110347143, -231.2371560537167170 ) ) ;
#1930 = VERTEX_POINT ( 'NONE', #13381 ) ;
#1931 = CARTESIAN_POINT ( 'NONE',  ( -11.96453848309674228, -6.796862595549911568, -223.8262896469332759 ) ) ;
#1932 = CARTESIAN_POINT ( 'NONE',  ( -5.861205904341304951, 14.21969934012253312, -219.3213214613830644 ) ) ;
#1933 = CARTESIAN_POINT ( 'NONE',  ( -2.270280637033633475, -14.48864307936496765, -230.4581659391201072 ) ) ;
#1934 = CARTESIAN_POINT ( 'NONE',  ( -7.189383125363055349, 14.28512618638020548, -231.7475838278701303 ) ) ;
#1935 = CARTESIAN_POINT ( 'NONE',  ( 5.326148043627311424, -14.37544986528147639, -217.4292808685971750 ) ) ;
#1936 = CARTESIAN_POINT ( 'NONE',  ( -23.14980455159086503, 0.3541108476526578785, -217.8785187302087536 ) ) ;
#1937 = CARTESIAN_POINT ( 'NONE',  ( -28.31595744342370580, 5.786754998807587924, -229.0820962600229223 ) ) ;
#1938 = CARTESIAN_POINT ( 'NONE',  ( -9.060146982536336324, 27.14942986116457746, -225.6568961786626062 ) ) ;
#1939 = CARTESIAN_POINT ( 'NONE',  ( -13.81390866287826746, 1.832988708064121175, -224.4361041349432639 ) ) ;
#1940 = CARTESIAN_POINT ( 'NONE',  ( -21.89065952084861522, -0.9940043559354512226, -215.0000000000000000 ) ) ;
#1941 = CARTESIAN_POINT ( 'NONE',  ( 15.15306935214909778, 7.771180183537883757, -217.5526096523957165 ) ) ;
#1942 = CARTESIAN_POINT ( 'NONE',  ( -0.1762641309874839746, -13.43768854674724977, -229.3744256026976416 ) ) ;
#1943 = CARTESIAN_POINT ( 'NONE',  ( 1.898427734299754421, 12.47096978853034521, -227.5043976727869506 ) ) ;
#1944 = TOROIDAL_SURFACE ( 'NONE', #16681, 22.63401512838748175, 3.000000000000002665 ) ;
#1945 = CARTESIAN_POINT ( 'NONE',  ( 20.89184612657454920, 5.404957034965973683, -232.0952743654565609 ) ) ;
#1946 = CARTESIAN_POINT ( 'NONE',  ( -7.274850400134849515, -18.40080456867533698, -234.8703629377345692 ) ) ;
#1947 = CARTESIAN_POINT ( 'NONE',  ( -8.857704405076667342, 24.20848540845601704, -218.8859504303524091 ) ) ;
#1948 = CARTESIAN_POINT ( 'NONE',  ( 5.702651035983461902, 12.42242820409033222, -224.7304266323218656 ) ) ;
#1949 = EDGE_CURVE ( 'NONE', #722, #21305, #10868, .T. ) ;
#1950 = CARTESIAN_POINT ( 'NONE',  ( -17.21167111787709914, -1.850592482912338799, -230.8442569545952665 ) ) ;
#1951 = CARTESIAN_POINT ( 'NONE',  ( -14.67397018911906770, 9.031553917454052893, -228.4349422195089119 ) ) ;
#1952 = CARTESIAN_POINT ( 'NONE',  ( -4.334570222994868161, 11.62786715207288601, -222.6396919303362267 ) ) ;
#1953 = CARTESIAN_POINT ( 'NONE',  ( 27.54521312182184545, 10.10774643363308023, -222.6232199463151744 ) ) ;
#1954 = ORIENTED_EDGE ( 'NONE', *, *, #3358, .F. ) ;
#1955 = CARTESIAN_POINT ( 'NONE',  ( 7.240923751923983964, -14.90955521745277501, -222.5312387745455283 ) ) ;
#1956 = VERTEX_POINT ( 'NONE', #18892 ) ;
#1957 = CARTESIAN_POINT ( 'NONE',  ( 11.29822263435752205, -11.23247557268489771, -230.2410575525588570 ) ) ;
#1958 = CARTESIAN_POINT ( 'NONE',  ( -3.130917144532865848, 26.01013079854885390, -229.4331404728494874 ) ) ;
#1959 = VERTEX_POINT ( 'NONE', #1782 ) ;
#1960 = CARTESIAN_POINT ( 'NONE',  ( 0.000000000000000000, 0.000000000000000000, -75.00000000000000000 ) ) ;
#1961 =( GEOMETRIC_REPRESENTATION_CONTEXT ( 3 ) GLOBAL_UNCERTAINTY_ASSIGNED_CONTEXT ( ( #19989 ) ) GLOBAL_UNIT_ASSIGNED_CONTEXT ( ( #1634, #15705, #7260 ) ) REPRESENTATION_CONTEXT ( 'NONE', 'WORKASPACE' ) );
#1962 = CARTESIAN_POINT ( 'NONE',  ( 14.31308345469695453, 12.76656023072872159, -231.9445021321040770 ) ) ;
#1963 = CARTESIAN_POINT ( 'NONE',  ( -30.62445638522240188, 0.2907099072661952222, -224.9999970559163387 ) ) ;
#1964 = CARTESIAN_POINT ( 'NONE',  ( -7.800954605602409053, -29.95157606033723496, -226.5906573908930000 ) ) ;
#1965 = CARTESIAN_POINT ( 'NONE',  ( 8.021672912688133650, -23.92397517040199872, -233.3380040120402441 ) ) ;
#1966 = CARTESIAN_POINT ( 'NONE',  ( -7.058999618647554541, 24.62458660126260312, -219.6630466582859356 ) ) ;
#1967 = DIRECTION ( 'NONE',  ( 0.000000000000000000, 0.000000000000000000, -1.000000000000000000 ) ) ;
#1968 = CARTESIAN_POINT ( 'NONE',  ( 12.91676121433235913, 9.519065828383201477, -226.8102878246443765 ) ) ;
#1969 = CARTESIAN_POINT ( 'NONE',  ( -3.326157069579807946, 13.92020081821418565, -220.5733722327383930 ) ) ;
#1970 = CARTESIAN_POINT ( 'NONE',  ( -13.96653539523557619, 20.94398119165846239, -231.8597527081015528 ) ) ;
#1971 = CARTESIAN_POINT ( 'NONE',  ( -3.494873682963683059, 27.70407912598904687, -220.5214894769905243 ) ) ;
#1972 = CARTESIAN_POINT ( 'NONE',  ( -19.67797246974518544, 1.229961341702398681, -219.4743747885323160 ) ) ;
#1973 = CARTESIAN_POINT ( 'NONE',  ( 11.20713200305815427, 28.28922876448651635, -219.1239564724620834 ) ) ;
#1974 = CARTESIAN_POINT ( 'NONE',  ( 13.17817051516727922, -26.22376201054615308, -223.3126545406654486 ) ) ;
#1975 = CARTESIAN_POINT ( 'NONE',  ( -16.23205080756887853, 1.987852906508643644E-15, 93.00000000000000000 ) ) ;
#1976 = EDGE_LOOP ( 'NONE', ( #12539, #12676 ) ) ;
#1977 = CARTESIAN_POINT ( 'NONE',  ( 1.773982976645536835, 19.12448993322812285, -233.2315972735944172 ) ) ;
#1978 = CARTESIAN_POINT ( 'NONE',  ( 16.24842259479558848, -3.494976385286828080, -222.6392560871376816 ) ) ;
#1979 = DIRECTION ( 'NONE',  ( 1.000000000000000000, 0.000000000000000000, 0.000000000000000000 ) ) ;
#1980 = CARTESIAN_POINT ( 'NONE',  ( 21.60524407607017849, 3.028118258437591415, -217.8361640396714449 ) ) ;
#1981 = CARTESIAN_POINT ( 'NONE',  ( -26.58771759052039485, 5.114955214121561511, -218.2823714869195442 ) ) ;
#1982 = CIRCLE ( 'NONE', #17819, 3.000000000000030198 ) ;
#1983 = CARTESIAN_POINT ( 'NONE',  ( 2.513843158659109456, -14.78137297724497401, -219.3443999184743518 ) ) ;
#1984 = CARTESIAN_POINT ( 'NONE',  ( -6.855867220396999251, 12.17758473459128332, -220.6375607554995213 ) ) ;
#1985 = ORIENTED_EDGE ( 'NONE', *, *, #15578, .T. ) ;
#1986 = CARTESIAN_POINT ( 'NONE',  ( -29.30406754532526037, 5.063969254119831120, -221.8212091093853076 ) ) ;
#1987 = CARTESIAN_POINT ( 'NONE',  ( -9.225692202065292946, -15.38374647092247116, -218.6784895636799320 ) ) ;
#1988 = CARTESIAN_POINT ( 'NONE',  ( 0.000000000000000000, 21.00000000000000000, 75.00000000000000000 ) ) ;
#1989 = CARTESIAN_POINT ( 'NONE',  ( -25.61997837663875188, 10.01664178086244483, -231.6711741719404074 ) ) ;
#1990 = CARTESIAN_POINT ( 'NONE',  ( 20.36520141328406552, -18.94542628267938156, -227.6082859645964902 ) ) ;
#1991 = CARTESIAN_POINT ( 'NONE',  ( 0.000000000000000000, 0.000000000000000000, 89.47905546699919910 ) ) ;
#1992 = CARTESIAN_POINT ( 'NONE',  ( -23.02469226963562576, 9.740049813577488891, -2.289467137130462238 ) ) ;
#1993 = CARTESIAN_POINT ( 'NONE',  ( 24.96615890023450035, 5.871290975262302148, -218.1661911638112201 ) ) ;
#1994 = EDGE_CURVE ( 'NONE', #6655, #4083, #3238, .T. ) ;
#1995 = CARTESIAN_POINT ( 'NONE',  ( -7.312583518931054627, 16.22063427959223958, -217.3454962955413521 ) ) ;
#1996 = CARTESIAN_POINT ( 'NONE',  ( 0.000000000000000000, 0.000000000000000000, -75.00000000000000000 ) ) ;
#1997 = CARTESIAN_POINT ( 'NONE',  ( 20.58393751692968721, 18.55948753678544705, -226.8933397075267635 ) ) ;
#1998 = CARTESIAN_POINT ( 'NONE',  ( 0.3267584840439746174, -16.39795729406718650, -220.1296710765888065 ) ) ;
#1999 = CARTESIAN_POINT ( 'NONE',  ( 26.13397685888192257, -0.5417465609251845837, -217.5756777990261526 ) ) ;
#2000 = ORIENTED_EDGE ( 'NONE', *, *, #16135, .T. ) ;
#2001 = CARTESIAN_POINT ( 'NONE',  ( 0.8374361358884788720, 23.73768315274483953, -232.4065959030912154 ) ) ;
#2002 = CARTESIAN_POINT ( 'NONE',  ( -16.58624905143161143, 8.715293938925766426, -220.0618460037763384 ) ) ;
#2003 = CARTESIAN_POINT ( 'NONE',  ( -25.59521542166570640, 7.637420400166985424, -216.4190921938142935 ) ) ;
#2004 = CARTESIAN_POINT ( 'NONE',  ( -14.51900513504577717, -8.991447007532661573, -221.0515111571761793 ) ) ;
#2005 = CARTESIAN_POINT ( 'NONE',  ( 26.00000000000000000, 0.000000000000000000, 0.000000000000000000 ) ) ;
#2006 = ORIENTED_EDGE ( 'NONE', *, *, #15250, .F. ) ;
#2007 = CARTESIAN_POINT ( 'NONE',  ( 27.84414217501293010, 2.965433895642837214, -221.8999927093654492 ) ) ;
#2008 = CARTESIAN_POINT ( 'NONE',  ( 0.4541713596374759021, -15.35025901140449989, -222.0332685144132370 ) ) ;
#2009 = CARTESIAN_POINT ( 'NONE',  ( 26.24002132888527328, 11.62331517472360964, -222.5300873157218859 ) ) ;
#2010 = CARTESIAN_POINT ( 'NONE',  ( -13.58874046263339608, 12.73011668665171392, -216.5659449791897941 ) ) ;
#2011 = CIRCLE ( 'NONE', #21053, 21.80000000000000071 ) ;
#2012 = CARTESIAN_POINT ( 'NONE',  ( 20.64287812348744566, 0.2024751443801864337, -216.7518974727033481 ) ) ;
#2013 =( GEOMETRIC_REPRESENTATION_CONTEXT ( 3 ) GLOBAL_UNCERTAINTY_ASSIGNED_CONTEXT ( ( #9656 ) ) GLOBAL_UNIT_ASSIGNED_CONTEXT ( ( #18358, #8125, #14991 ) ) REPRESENTATION_CONTEXT ( 'NONE', 'WORKASPACE' ) );
#2014 = CARTESIAN_POINT ( 'NONE',  ( 5.141746912158045468, 22.01688500372448232, -216.6678693612369386 ) ) ;
#2015 = CARTESIAN_POINT ( 'NONE',  ( 14.15986309589296788, 2.061458568213107245, -222.8204610720217147 ) ) ;
#2016 = CARTESIAN_POINT ( 'NONE',  ( -1.608171596096409806, -16.77465153034988887, -217.4618546331240054 ) ) ;
#2017 = CARTESIAN_POINT ( 'NONE',  ( 25.69672030403964769, -15.30292110028031338, -224.0206579222720791 ) ) ;
#2018 = DIRECTION ( 'NONE',  ( 1.000000000000000000, 0.000000000000000000, 0.000000000000000000 ) ) ;
#2019 = FACE_OUTER_BOUND ( 'NONE', #6808, .T. ) ;
#2020 = CARTESIAN_POINT ( 'NONE',  ( -7.399925907206128528, 10.29859031525428037, -227.1614041762800298 ) ) ;
#2021 = CARTESIAN_POINT ( 'NONE',  ( -25.38303270991942284, -1.762464254583185452, -219.8781034644853776 ) ) ;
#2022 = CARTESIAN_POINT ( 'NONE',  ( 29.47107563651793427, 6.731311671946880182, -220.0565342412898815 ) ) ;
#2023 = CARTESIAN_POINT ( 'NONE',  ( 0.3632086708616291126, 21.06287758167331958, -232.5112839711303820 ) ) ;
#2024 = CARTESIAN_POINT ( 'NONE',  ( 5.142103055192286831, 28.18228231877369439, -225.8998064704803994 ) ) ;
#2025 = ORIENTED_EDGE ( 'NONE', *, *, #1211, .T. ) ;
#2026 = CARTESIAN_POINT ( 'NONE',  ( 9.181101971147782592, -9.127577137574531818, -229.3209091633710273 ) ) ;
#2027 = VERTEX_POINT ( 'NONE', #10233 ) ;
#2028 = CIRCLE ( 'NONE', #16770, 23.92685091328691271 ) ;
#2029 = CARTESIAN_POINT ( 'NONE',  ( 19.19288224840068935, 10.13059690604263174, -232.1906135022504998 ) ) ;
#2030 = CARTESIAN_POINT ( 'NONE',  ( -14.58670098223046629, 7.239570004716886942, -229.3284954533748135 ) ) ;
#2031 = CARTESIAN_POINT ( 'NONE',  ( -21.66801938871533650, 16.28801167444048659, -218.5240035253498547 ) ) ;
#2032 = CARTESIAN_POINT ( 'NONE',  ( -30.78084016402396372, -2.501288241119758116, -224.5721874330603214 ) ) ;
#2033 = CARTESIAN_POINT ( 'NONE',  ( -10.65455960636934662, 10.37188583052882862, -219.5197110153079620 ) ) ;
#2034 = CARTESIAN_POINT ( 'NONE',  ( 1.387778780781446180E-13, -19.80000000000006111, -78.50000000000000000 ) ) ;
#2035 = CARTESIAN_POINT ( 'NONE',  ( 14.88115968084168728, -2.531949626111721585, -226.6122033079182074 ) ) ;
#2036 = CARTESIAN_POINT ( 'NONE',  ( 22.36788034568564854, -2.140002702436959225, -217.7104380410378610 ) ) ;
#2037 = DIRECTION ( 'NONE',  ( -0.000000000000000000, -1.000000000000000000, -0.000000000000000000 ) ) ;
#2038 = EDGE_CURVE ( 'NONE', #11804, #19581, #442, .T. ) ;
#2039 = CARTESIAN_POINT ( 'NONE',  ( -11.83954511762131112, 10.58068896997146346, -226.6171226499791089 ) ) ;
#2040 = CARTESIAN_POINT ( 'NONE',  ( 12.58033168766476528, 20.35631482982274676, -235.1670639654690547 ) ) ;
#2041 = CARTESIAN_POINT ( 'NONE',  ( -16.15126510923403202, -0.4755054218165427615, -219.3066569788202571 ) ) ;
#2042 = CARTESIAN_POINT ( 'NONE',  ( -28.75820353979175081, -10.31764292692039753, -230.8958203355234389 ) ) ;
#2043 = CARTESIAN_POINT ( 'NONE',  ( -25.32486352395475393, -3.505876693931964549, -233.0869506614649822 ) ) ;
#2044 = CARTESIAN_POINT ( 'NONE',  ( -23.16143087541734502, 21.36835206473086046, -221.8715256527013651 ) ) ;
#2045 = CARTESIAN_POINT ( 'NONE',  ( -11.06377138986482933, -15.30386857868810857, -217.0411070525910873 ) ) ;
#2046 = CARTESIAN_POINT ( 'NONE',  ( 17.68508104102419409, 23.41266195669770767, -227.5327139115408954 ) ) ;
#2047 = CARTESIAN_POINT ( 'NONE',  ( 3.531840179394873491, -11.29480931768500618, -224.5922842895475355 ) ) ;
#2048 = DIRECTION ( 'NONE',  ( 1.000000000000000000, -0.000000000000000000, -0.000000000000000000 ) ) ;
#2049 = CARTESIAN_POINT ( 'NONE',  ( 12.43753614017300713, 2.441361880258234862, -222.2750447601761721 ) ) ;
#2050 = CARTESIAN_POINT ( 'NONE',  ( -2.612157044224189484, 27.88031182936952135, -224.5292183073761692 ) ) ;
#2051 = CARTESIAN_POINT ( 'NONE',  ( -24.15814485343234352, 4.373587128574028426, -232.6698675874553430 ) ) ;
#2052 = CARTESIAN_POINT ( 'NONE',  ( 15.42212722119060864, 5.401662248084913465, -220.8333402320903645 ) ) ;
#2053 = CARTESIAN_POINT ( 'NONE',  ( 15.89621445970763070, 6.639162626453350313, -232.5295318698041456 ) ) ;
#2054 = CARTESIAN_POINT ( 'NONE',  ( -9.132447960227011663, -28.48575439045284696, -228.2342138548108892 ) ) ;
#2055 = CARTESIAN_POINT ( 'NONE',  ( 10.22554538262735413, 24.20440706210576209, -215.6176527921760737 ) ) ;
#2056 = LINE ( 'NONE', #5422, #9459 ) ;
#2057 = CARTESIAN_POINT ( 'NONE',  ( -14.97068153222459408, -28.62142063984003215, -225.0224449979507142 ) ) ;
#2058 = CARTESIAN_POINT ( 'NONE',  ( -7.375127652145912371, 13.01042140126078195, -223.9959097520547004 ) ) ;
#2059 = CARTESIAN_POINT ( 'NONE',  ( 11.96568375430165254, 8.504117401580989721, -219.8633768076029753 ) ) ;
#2060 = CARTESIAN_POINT ( 'NONE',  ( -29.27492217116574480, -1.185422171198730501, -224.8132346143397342 ) ) ;
#2061 = CARTESIAN_POINT ( 'NONE',  ( -17.75632171729475317, 14.45153669854845901, -218.6240360064753929 ) ) ;
#2062 = CARTESIAN_POINT ( 'NONE',  ( -9.251743101293765648, 14.06372330290396278, -232.4239003576353468 ) ) ;
#2063 = CARTESIAN_POINT ( 'NONE',  ( 15.92396645628901020, -0.3225394686005420009, -223.0199929375764327 ) ) ;
#2064 = VERTEX_POINT ( 'NONE', #20223 ) ;
#2065 = CARTESIAN_POINT ( 'NONE',  ( 6.629309777743229937, -15.42610274396934855, -227.9597969125812256 ) ) ;
#2066 = CARTESIAN_POINT ( 'NONE',  ( 13.07616324839670341, -23.69356132834180784, -230.7206382488779184 ) ) ;
#2067 = CARTESIAN_POINT ( 'NONE',  ( -2.618694198633108261, 15.69630225547860825, -226.1451761977223498 ) ) ;
#2068 = ORIENTED_EDGE ( 'NONE', *, *, #1832, .F. ) ;
#2069 = DIRECTION ( 'NONE',  ( -0.000000000000000000, 0.000000000000000000, -1.000000000000000000 ) ) ;
#2070 = CARTESIAN_POINT ( 'NONE',  ( 16.54345861550681107, 19.37554510112122230, -218.2240151908141002 ) ) ;
#2071 = CARTESIAN_POINT ( 'NONE',  ( -13.18205254385204661, -0.5588607053421433823, -223.2849229087554761 ) ) ;
#2072 = CARTESIAN_POINT ( 'NONE',  ( -25.82802808205240552, -14.78441951539553401, -222.6940535085979604 ) ) ;
#2073 = CARTESIAN_POINT ( 'NONE',  ( 7.486336813247038258, -29.35413437595724773, -221.4114973598149447 ) ) ;
#2074 = CARTESIAN_POINT ( 'NONE',  ( -5.600903697806950632, 21.62055466701630735, -218.6671277943675307 ) ) ;
#2075 = DIRECTION ( 'NONE',  ( -1.000000000000000000, 0.000000000000000000, 0.000000000000000000 ) ) ;
#2076 = CARTESIAN_POINT ( 'NONE',  ( 18.51425713624010427, 11.82474821235740592, -231.3645840199355632 ) ) ;
#2077 = CARTESIAN_POINT ( 'NONE',  ( -11.42613629117093765, 28.09170287990588832, -228.7150250545069241 ) ) ;
#2078 = CARTESIAN_POINT ( 'NONE',  ( -6.901278853520646628, 15.41233971300566807, -220.5972764307651346 ) ) ;
#2079 = ORIENTED_EDGE ( 'NONE', *, *, #3880, .F. ) ;
#2080 = EDGE_CURVE ( 'NONE', #10588, #846, #3065, .T. ) ;
#2081 = CARTESIAN_POINT ( 'NONE',  ( 2.808299412262623473, 18.06245856371233316, -217.9832661743849656 ) ) ;
#2082 = CARTESIAN_POINT ( 'NONE',  ( -15.82760502346409304, 5.624826830110399634, -227.5369622385896946 ) ) ;
#2083 = CARTESIAN_POINT ( 'NONE',  ( 27.08260752785270853, 4.114838227474355570, -232.2882281786467331 ) ) ;
#2084 = CARTESIAN_POINT ( 'NONE',  ( 5.380811198380419214, -14.52623441703906160, -221.9013399998540024 ) ) ;
#2085 = CARTESIAN_POINT ( 'NONE',  ( 2.000000000000000000, 0.000000000000000000, -120.0000000000000142 ) ) ;
#2086 = ORIENTED_EDGE ( 'NONE', *, *, #21351, .F. ) ;
#2087 = CARTESIAN_POINT ( 'NONE',  ( 4.343013938751969505, 13.02036404005131587, -224.7825435359082178 ) ) ;
#2088 = CARTESIAN_POINT ( 'NONE',  ( 24.96598054343045447, -3.653363829669123319, -219.8248103142179559 ) ) ;
#2089 = DIRECTION ( 'NONE',  ( 1.000000000000000000, 0.000000000000000000, 0.000000000000000000 ) ) ;
#2090 = CARTESIAN_POINT ( 'NONE',  ( 22.86997486125673618, 17.56009411325475966, -222.3578648042903296 ) ) ;
#2091 = CARTESIAN_POINT ( 'NONE',  ( 12.73130673999417795, -23.76414828096303467, -217.7386337832039942 ) ) ;
#2092 = CARTESIAN_POINT ( 'NONE',  ( 0.000000000000000000, 0.000000000000000000, 0.000000000000000000 ) ) ;
#2093 = CARTESIAN_POINT ( 'NONE',  ( -16.39453490553961856, 20.24836633112041184, -233.1722131570092245 ) ) ;
#2094 = CARTESIAN_POINT ( 'NONE',  ( -19.58639255110637478, 14.91076398872931819, -217.1105532241463720 ) ) ;
#2095 = CARTESIAN_POINT ( 'NONE',  ( 20.54442553493903389, -1.409480604460696007, -231.2888200459364327 ) ) ;
#2096 = CARTESIAN_POINT ( 'NONE',  ( -16.38803511840525218, -9.809678413005567421, -217.1940421839195494 ) ) ;
#2097 = DIRECTION ( 'NONE',  ( -6.982962677686272233E-15, 1.000000000000000000, 0.000000000000000000 ) ) ;
#2098 = DIRECTION ( 'NONE',  ( 0.000000000000000000, 0.000000000000000000, -1.000000000000000000 ) ) ;
#2099 = CARTESIAN_POINT ( 'NONE',  ( -22.47200958260654957, 4.697452857301940732, -216.5879371680706242 ) ) ;
#2100 = CARTESIAN_POINT ( 'NONE',  ( 0.2152704783746036410, -12.84635275796930642, -226.1081088095504015 ) ) ;
#2101 = SURFACE_SIDE_STYLE ('',( #15737 ) ) ;
#2102 = CARTESIAN_POINT ( 'NONE',  ( -24.65444200344273895, 4.153573317486630501, 9.102483954860396409 ) ) ;
#2103 = CARTESIAN_POINT ( 'NONE',  ( 24.93482953594869755, 13.13888391581411241, -222.4369546851285691 ) ) ;
#2104 = CARTESIAN_POINT ( 'NONE',  ( -21.64120863631820413, 17.87363223393748868, -233.1390268986752119 ) ) ;
#2105 = VECTOR ( 'NONE', #3987, 1000.000000000000000 ) ;
#2106 = DIRECTION ( 'NONE',  ( 0.000000000000000000, 0.000000000000000000, -1.000000000000000000 ) ) ;
#2107 = CARTESIAN_POINT ( 'NONE',  ( 20.92326490933994876, 18.00580109995737033, -222.6060933800056034 ) ) ;
#2108 = CARTESIAN_POINT ( 'NONE',  ( -0.5904090961472509003, -15.19049578300894510, -228.4387523405810612 ) ) ;
#2109 = EDGE_CURVE ( 'NONE', #8590, #10116, #1512, .T. ) ;
#2110 = ORIENTED_EDGE ( 'NONE', *, *, #15578, .F. ) ;
#2111 = CARTESIAN_POINT ( 'NONE',  ( -1.772400894765090662, 19.49811434610897010, -217.8797837662441168 ) ) ;
#2112 = CARTESIAN_POINT ( 'NONE',  ( -8.985448925281199095, 11.82743561134668475, -224.1067108988273162 ) ) ;
#2113 = CARTESIAN_POINT ( 'NONE',  ( -29.98527381603928887, 6.316825171121390525, -230.1108345570740994 ) ) ;
#2114 = CARTESIAN_POINT ( 'NONE',  ( -13.68888474783054399, -8.264665463295720826, -223.0168115903771024 ) ) ;
#2115 = DIRECTION ( 'NONE',  ( -1.000000000000000000, 0.000000000000000000, 0.000000000000000000 ) ) ;
#2116 = EDGE_LOOP ( 'NONE', ( #95, #7084, #17209, #11400 ) ) ;
#2117 = CARTESIAN_POINT ( 'NONE',  ( 12.91815243135930480, 5.607966342865584153, -224.2227256053222959 ) ) ;
#2118 = CARTESIAN_POINT ( 'NONE',  ( 6.833096512853454207, -24.74801519961247465, -219.7405977492105364 ) ) ;
#2119 = CARTESIAN_POINT ( 'NONE',  ( 15.87442104186276381, 8.674488492264579520, -230.9702037640878416 ) ) ;
#2120 = CARTESIAN_POINT ( 'NONE',  ( -12.90983082593748676, 14.84936372681532823, -233.8009687022269532 ) ) ;
#2121 = ADVANCED_FACE ( 'NONE', ( #13615 ), #20452, .T. ) ;
#2122 = CARTESIAN_POINT ( 'NONE',  ( 22.17049319811867036, 0.5483778423327810847, -216.5715983009590673 ) ) ;
#2123 = CARTESIAN_POINT ( 'NONE',  ( 4.354034006296288339, 14.09944204372416188, -221.2519525881239417 ) ) ;
#2124 = CARTESIAN_POINT ( 'NONE',  ( -10.75744069813302417, 0.6349943332661998063, 92.00000000000000000 ) ) ;
#2125 = EDGE_CURVE ( 'NONE', #3502, #10973, #8356, .T. ) ;
#2126 = CARTESIAN_POINT ( 'NONE',  ( -6.722478243781921492, -14.20656108661463612, -231.4169491518476889 ) ) ;
#2127 = CARTESIAN_POINT ( 'NONE',  ( 16.07085865561684201, -17.65509622858733252, -216.6880805489183501 ) ) ;
#2128 = DIRECTION ( 'NONE',  ( 0.000000000000000000, 0.000000000000000000, 1.000000000000000000 ) ) ;
#2129 = DIRECTION ( 'NONE',  ( -0.000000000000000000, -0.000000000000000000, -1.000000000000000000 ) ) ;
#2130 = CARTESIAN_POINT ( 'NONE',  ( -9.964021556040458805, 12.25789996591640119, -217.8262340283327774 ) ) ;
#2131 = CARTESIAN_POINT ( 'NONE',  ( -16.09622215267033596, -6.362375831002168525, -228.5323951500822943 ) ) ;
#2132 = CARTESIAN_POINT ( 'NONE',  ( -14.69827142695382527, 14.49176359921644597, -217.9600391472806109 ) ) ;
#2133 = CARTESIAN_POINT ( 'NONE',  ( 3.312424284731937618, 15.29837714273186045, -229.5209971419123747 ) ) ;
#2134 = CARTESIAN_POINT ( 'NONE',  ( 5.112468059216026539, 15.05346046978967856, -223.6558835435016590 ) ) ;
#2135 = ORIENTED_EDGE ( 'NONE', *, *, #12683, .T. ) ;
#2136 = CARTESIAN_POINT ( 'NONE',  ( 9.167096742983094515, -14.53852251116023986, -217.0563232478103828 ) ) ;
#2137 = ORIENTED_EDGE ( 'NONE', *, *, #15468, .T. ) ;
#2138 = CARTESIAN_POINT ( 'NONE',  ( 24.58316096239279602, 5.861425670879941485, -231.3104446318280623 ) ) ;
#2139 = CARTESIAN_POINT ( 'NONE',  ( -7.752954785937490989, 10.21341112307795385, -225.5135920495299615 ) ) ;
#2140 = CARTESIAN_POINT ( 'NONE',  ( -15.61959985466312872, 8.133362592386543355, -230.7826037412100106 ) ) ;
#2141 = CARTESIAN_POINT ( 'NONE',  ( -24.78729321827560739, -16.46449136890227294, -222.3867555963062443 ) ) ;
#2142 = CARTESIAN_POINT ( 'NONE',  ( -27.82842955277035202, 11.70195273568964112, -227.9294339757464911 ) ) ;
#2143 = CARTESIAN_POINT ( 'NONE',  ( 0.000000000000000000, 0.000000000000000000, 93.00000000000000000 ) ) ;
#2144 = CARTESIAN_POINT ( 'NONE',  ( 21.52074627118099315, 8.791036694007010155, -215.9547738671300294 ) ) ;
#2145 = CARTESIAN_POINT ( 'NONE',  ( -18.64931821476190876, 22.04453097546810270, -226.2485927806324923 ) ) ;
#2146 = CARTESIAN_POINT ( 'NONE',  ( 18.26039090677515375, 26.14311541888654844, -228.1864986152887127 ) ) ;
#2147 = CARTESIAN_POINT ( 'NONE',  ( -13.11494368899652052, 3.355507568391938200, -225.9121440085824304 ) ) ;
#2148 = CARTESIAN_POINT ( 'NONE',  ( -23.48355816166749932, -5.921172941748132246, -214.8630305010649408 ) ) ;
#2149 = CARTESIAN_POINT ( 'NONE',  ( -25.34460520202507539, -7.988444519707189606, -217.6292756219348234 ) ) ;
#2150 = CARTESIAN_POINT ( 'NONE',  ( -1.946052076048385482, 22.23149728939677061, -232.8927760318659068 ) ) ;
#2151 = CARTESIAN_POINT ( 'NONE',  ( -6.012234575298915473, -13.00555924700598709, -229.4955436083688483 ) ) ;
#2152 = CARTESIAN_POINT ( 'NONE',  ( 6.093530912645064745, 16.79941505724243811, -232.1766444656230419 ) ) ;
#2153 = CARTESIAN_POINT ( 'NONE',  ( 8.798770371347417907, -12.71349942585338333, -232.9159113209695704 ) ) ;
#2154 = FACE_BOUND ( 'NONE', #18087, .T. ) ;
#2155 = CARTESIAN_POINT ( 'NONE',  ( 13.98152565379061052, 2.156981915107639036, -230.5667344709999611 ) ) ;
#2156 = DIRECTION ( 'NONE',  ( -0.000000000000000000, -1.000000000000000000, -0.000000000000000000 ) ) ;
#2157 = CARTESIAN_POINT ( 'NONE',  ( -0.6272116608575281083, 20.18031380156121202, -219.3960054794027030 ) ) ;
#2158 = CARTESIAN_POINT ( 'NONE',  ( -22.13857085231108712, 6.545953331035805789, -217.2801712530867633 ) ) ;
#2159 = CARTESIAN_POINT ( 'NONE',  ( 20.23125423326388628, 7.836699765464857137, -217.8891354894872450 ) ) ;
#2160 = CARTESIAN_POINT ( 'NONE',  ( 16.73391517716289911, 11.95167056011791828, -233.0268722588312755 ) ) ;
#2161 = CARTESIAN_POINT ( 'NONE',  ( -14.39178795515995724, -23.41959061255243313, -230.2514514786898019 ) ) ;
#2162 = CARTESIAN_POINT ( 'NONE',  ( 2.987882271643250931, 28.57355997650491020, -217.8917278841813925 ) ) ;
#2163 = DIRECTION ( 'NONE',  ( 0.000000000000000000, 0.000000000000000000, 1.000000000000000000 ) ) ;
#2164 = CARTESIAN_POINT ( 'NONE',  ( -11.40836237951390508, -18.42461209671423816, -214.6264694599774430 ) ) ;
#2165 = CARTESIAN_POINT ( 'NONE',  ( -4.466732464217805898, 19.42663028452474450, -231.9485309169485561 ) ) ;
#2166 = CARTESIAN_POINT ( 'NONE',  ( 14.63115627273841923, 9.024791562541032874, -232.5054678133655841 ) ) ;
#2167 = CARTESIAN_POINT ( 'NONE',  ( -21.10507617219916199, 14.90539259013048756, -229.7677326419877488 ) ) ;
#2168 = CLOSED_SHELL ( 'NONE', ( #876, #15317, #2802, #6387, #3276, #20231, #8918, #6260, #11075, #12311, #16542, #17405, #7759, #13941 ) ) ;
#2169 = CARTESIAN_POINT ( 'NONE',  ( -4.695076324262313250, 31.85502299853856201, -223.8918597786031341 ) ) ;
#2170 = AXIS2_PLACEMENT_3D ( 'NONE', #8967, #408, #3883 ) ;
#2171 = CARTESIAN_POINT ( 'NONE',  ( 19.87150736056128864, 8.436445599727830924, -233.0166429845654932 ) ) ;
#2172 = CARTESIAN_POINT ( 'NONE',  ( 17.47473467751515486, -18.15791173363047051, -230.0427332633545632 ) ) ;
#2173 = CARTESIAN_POINT ( 'NONE',  ( 15.50624253654579654, -15.96056326703506478, -233.0338314371582840 ) ) ;
#2174 = CARTESIAN_POINT ( 'NONE',  ( -2.532302712337851425, 16.54370602006230939, -228.1940632970506613 ) ) ;
#2175 = DIRECTION ( 'NONE',  ( 1.000000000000000000, 0.000000000000000000, 0.000000000000000000 ) ) ;
#2176 = CARTESIAN_POINT ( 'NONE',  ( 17.19674704922021391, 23.07334190050143974, -228.8256488842130238 ) ) ;
#2177 = CARTESIAN_POINT ( 'NONE',  ( -16.32911940539174367, -0.4850290419235887551, -232.0399150213553412 ) ) ;
#2178 = CARTESIAN_POINT ( 'NONE',  ( -15.58529874627549461, -6.917566422457355202, -219.0138643999995054 ) ) ;
#2179 = CARTESIAN_POINT ( 'NONE',  ( 4.201723131641114328, -20.76291977712905279, -215.9522215885928347 ) ) ;
#2180 = CARTESIAN_POINT ( 'NONE',  ( -6.769588938507062004, 18.22485903270490937, -231.3660928915624879 ) ) ;
#2181 = DIRECTION ( 'NONE',  ( -0.000000000000000000, -0.000000000000000000, -1.000000000000000000 ) ) ;
#2182 = CARTESIAN_POINT ( 'NONE',  ( 17.42772712443221650, 11.35756022693713341, -231.2166398222404382 ) ) ;
#2183 = CARTESIAN_POINT ( 'NONE',  ( -11.24282496690421596, 12.44430180464951086, -232.4405891940542404 ) ) ;
#2184 = CARTESIAN_POINT ( 'NONE',  ( -10.52776196018457711, 13.57482816453351937, -219.2327734183297423 ) ) ;
#2185 = ORIENTED_EDGE ( 'NONE', *, *, #9624, .T. ) ;
#2186 = CARTESIAN_POINT ( 'NONE',  ( 10.25948093768852054, 28.38842464930171872, -224.3436940787075855 ) ) ;
#2187 = CARTESIAN_POINT ( 'NONE',  ( -20.21481434941064848, 7.972326285609216967, -230.8475376972877484 ) ) ;
#2188 = CARTESIAN_POINT ( 'NONE',  ( 29.21307215008108216, 4.139194015751272104, -229.9658791484231699 ) ) ;
#2189 = CARTESIAN_POINT ( 'NONE',  ( 4.725966861008204845, -14.24791254766627624, -227.2781441550517343 ) ) ;
#2190 = DIRECTION ( 'NONE',  ( 0.000000000000000000, -1.000000000000000000, 0.000000000000000000 ) ) ;
#2191 = ORIENTED_EDGE ( 'NONE', *, *, #18360, .T. ) ;
#2192 = ADVANCED_FACE ( 'NONE', ( #8994 ), #7283, .T. ) ;
#2193 = CARTESIAN_POINT ( 'NONE',  ( 7.995304978256253747, 13.28024228361502779, -220.6535174700288451 ) ) ;
#2194 = CARTESIAN_POINT ( 'NONE',  ( 28.03541074264261113, -3.118360251426135488, -224.4433144283077581 ) ) ;
#2195 = DIRECTION ( 'NONE',  ( -1.000000000000000000, 0.000000000000000000, 0.000000000000000000 ) ) ;
#2196 = CARTESIAN_POINT ( 'NONE',  ( 20.58703255433590940, 0.4816031003617209372, -231.9427175861361263 ) ) ;
#2197 = CARTESIAN_POINT ( 'NONE',  ( 1.127544764349826867, -27.89617517048659323, -231.9509945439240823 ) ) ;
#2198 = CARTESIAN_POINT ( 'NONE',  ( -18.09776816382430908, 23.50806826204562583, -229.9568677523880638 ) ) ;
#2199 = CARTESIAN_POINT ( 'NONE',  ( -13.31245686955614005, 26.96290519511623174, -230.1796856776773836 ) ) ;
#2200 = ORIENTED_EDGE ( 'NONE', *, *, #7776, .F. ) ;
#2201 = CARTESIAN_POINT ( 'NONE',  ( -24.68906941503829700, 2.445024713909649705, -232.6803430500543755 ) ) ;
#2202 = CARTESIAN_POINT ( 'NONE',  ( -8.978805095734141872, -14.89723076936793156, -219.0730636071341451 ) ) ;
#2203 = DIRECTION ( 'NONE',  ( -0.000000000000000000, -0.000000000000000000, 1.000000000000000000 ) ) ;
#2204 = DIRECTION ( 'NONE',  ( -1.000000000000000000, -1.224646799147353454E-16, 0.000000000000000000 ) ) ;
#2205 = CARTESIAN_POINT ( 'NONE',  ( -24.48580119005125866, 9.312492396273500006, -232.5498413856076070 ) ) ;
#2206 = CARTESIAN_POINT ( 'NONE',  ( -0.6133843921297743584, -15.86829592205942419, -231.9438830533787268 ) ) ;
#2207 = CARTESIAN_POINT ( 'NONE',  ( 1.387778780781445676E-13, -19.79999999999999716, -78.50000000000000000 ) ) ;
#2208 = CARTESIAN_POINT ( 'NONE',  ( -25.00000000000000000, -1.002884296170500229E-19, 10.00000000000000000 ) ) ;
#2209 = CARTESIAN_POINT ( 'NONE',  ( 14.37653162493774239, 9.985418694807894013, -229.1686718965858063 ) ) ;
#2210 = CARTESIAN_POINT ( 'NONE',  ( -5.607934827417612844, 15.68271927908880770, -232.1026723719274969 ) ) ;
#2211 = CARTESIAN_POINT ( 'NONE',  ( 1.232595164407830946E-29, -17.50000000000007105, -30.00000000000000000 ) ) ;
#2212 = CARTESIAN_POINT ( 'NONE',  ( 21.07144422417032104, 18.33581350331571969, -223.6711752364813890 ) ) ;
#2213 = CARTESIAN_POINT ( 'NONE',  ( -1.686103422391260764, -28.85289795882446029, -227.6662241409997876 ) ) ;
#2214 = ORIENTED_EDGE ( 'NONE', *, *, #11959, .F. ) ;
#2215 = CARTESIAN_POINT ( 'NONE',  ( -1.038524475621362075, 14.89017051181998141, -222.3948816610352139 ) ) ;
#2216 = CARTESIAN_POINT ( 'NONE',  ( -12.33583941212908108, 22.27382123621224608, -231.6290720151527296 ) ) ;
#2217 = CARTESIAN_POINT ( 'NONE',  ( -21.07387565400155438, 1.107905485989369554, -215.0000000023499069 ) ) ;
#2218 = TOROIDAL_SURFACE ( 'NONE', #7979, 24.63401512838747820, 3.000000000000000888 ) ;
#2219 = ORIENTED_EDGE ( 'NONE', *, *, #4940, .T. ) ;
#2220 = CARTESIAN_POINT ( 'NONE',  ( -13.03991958801536555, -12.43893258430110471, -220.5791972147702040 ) ) ;
#2221 = DIRECTION ( 'NONE',  ( -1.000000000000000000, 0.000000000000000000, 0.000000000000000000 ) ) ;
#2222 = ORIENTED_EDGE ( 'NONE', *, *, #12958, .T. ) ;
#2223 = CARTESIAN_POINT ( 'NONE',  ( -29.88125065636863198, 4.504452993877526623, -226.2048141718237275 ) ) ;
#2224 = CARTESIAN_POINT ( 'NONE',  ( 8.343784211782431015, -26.96289276196324636, -225.6651636531778422 ) ) ;
#2225 = CARTESIAN_POINT ( 'NONE',  ( 11.62313423782632782, 11.98467543564608029, -219.7293303032897995 ) ) ;
#2226 = CARTESIAN_POINT ( 'NONE',  ( 1.773982976645536835, 19.12448993322812285, -233.2315972735944172 ) ) ;
#2227 = UNCERTAINTY_MEASURE_WITH_UNIT (LENGTH_MEASURE( 1.000000000000000082E-05 ), #7286, 'distance_accuracy_value', 'NONE');
#2228 = CIRCLE ( 'NONE', #17321, 3.000000000000002665 ) ;
#2229 = CARTESIAN_POINT ( 'NONE',  ( 29.00474534066713872, 11.29707752057770698, -221.8682176444242771 ) ) ;
#2230 = EDGE_CURVE ( 'NONE', #9583, #1422, #18773, .T. ) ;
#2231 = CIRCLE ( 'NONE', #4373, 12.50000000000000355 ) ;
#2232 = CARTESIAN_POINT ( 'NONE',  ( 7.639528166734322667, 11.92751229241157596, -224.6077814063189635 ) ) ;
#2233 = PLANE ( 'NONE',  #13796 ) ;
#2234 = CARTESIAN_POINT ( 'NONE',  ( -8.379125946468517938, -29.31735857037017468, -221.8060643354269814 ) ) ;
#2235 = CARTESIAN_POINT ( 'NONE',  ( 24.05826999138443156, -14.97270453765939102, -220.1026142722873260 ) ) ;
#2236 = DIRECTION ( 'NONE',  ( 0.000000000000000000, 0.000000000000000000, -1.000000000000000000 ) ) ;
#2237 = CARTESIAN_POINT ( 'NONE',  ( -9.503027668167838726, 6.959046566381404730, -225.7241663910276941 ) ) ;
#2238 = CARTESIAN_POINT ( 'NONE',  ( -21.34127571194312623, -5.850660018714998856, -219.1209233896074977 ) ) ;
#2239 = EDGE_CURVE ( 'NONE', #17987, #10013, #9076, .T. ) ;
#2240 = CARTESIAN_POINT ( 'NONE',  ( -14.57944476639264764, 6.129437248167259433, -229.4766146696829310 ) ) ;
#2241 = CARTESIAN_POINT ( 'NONE',  ( 12.95792863868717149, 16.83236386576623644, -216.3406066345214356 ) ) ;
#2242 = CARTESIAN_POINT ( 'NONE',  ( 6.332229114051408203, 16.75791367489523154, -229.7702805136205200 ) ) ;
#2243 = ORIENTED_EDGE ( 'NONE', *, *, #15304, .F. ) ;
#2244 = CARTESIAN_POINT ( 'NONE',  ( 11.13603681652449318, -5.602932040673746172, -228.8141337797931101 ) ) ;
#2245 = ORIENTED_EDGE ( 'NONE', *, *, #11193, .T. ) ;
#2246 = CARTESIAN_POINT ( 'NONE',  ( 20.89184612657454920, 5.404957034965973683, -232.0952743654565609 ) ) ;
#2247 = CIRCLE ( 'NONE', #20205, 3.000000000000002665 ) ;
#2248 = AXIS2_PLACEMENT_3D ( 'NONE', #5502, #17450, #10466 ) ;
#2249 = CARTESIAN_POINT ( 'NONE',  ( -10.30034651166687887, 25.05454868506992838, -216.5587736482213188 ) ) ;
#2250 = CARTESIAN_POINT ( 'NONE',  ( -12.98662328632235585, 28.83726371277012035, -223.5970274767108776 ) ) ;
#2251 = CARTESIAN_POINT ( 'NONE',  ( -18.41550138691291139, -5.273244084890690075, -216.7348800533310964 ) ) ;
#2252 = CARTESIAN_POINT ( 'NONE',  ( -12.44873260470819787, 7.411970124596155785, -229.4214091473984070 ) ) ;
#2253 = LINE ( 'NONE', #19025, #11202 ) ;
#2254 = CARTESIAN_POINT ( 'NONE',  ( 27.02029988085337919, -0.4174685747284823112, -230.1188858631967378 ) ) ;
#2255 = CARTESIAN_POINT ( 'NONE',  ( -18.67270963783218463, 15.11229250701181925, -218.9067109956068578 ) ) ;
#2256 = CARTESIAN_POINT ( 'NONE',  ( 14.54999166170408209, 3.068772298969228096, -219.4784171371563275 ) ) ;
#2257 = CARTESIAN_POINT ( 'NONE',  ( 24.32561047128371001, 1.769413244618101011, -218.8629106451077462 ) ) ;
#2258 = CARTESIAN_POINT ( 'NONE',  ( 10.83706092800007781, 10.12544885278926543, -227.1716144446442343 ) ) ;
#2259 = AXIS2_PLACEMENT_3D ( 'NONE', #13081, #18367, #16564 ) ;
#2260 = CARTESIAN_POINT ( 'NONE',  ( -13.36955836198420577, -3.222265253903016990, -227.4060678739157026 ) ) ;
#2261 = CARTESIAN_POINT ( 'NONE',  ( -1.243734262319729389, 14.23902626181890518, -226.4313640849764795 ) ) ;
#2262 = CARTESIAN_POINT ( 'NONE',  ( 0.7326557587344989519, -29.96088689026728602, -229.4725774697800205 ) ) ;
#2263 = CARTESIAN_POINT ( 'NONE',  ( 10.02513374692848913, 18.81568788741115128, -217.1505009242214612 ) ) ;
#2264 = CARTESIAN_POINT ( 'NONE',  ( 6.835279263914467052, -26.27742004305391177, -233.7345821414606348 ) ) ;
#2265 = CARTESIAN_POINT ( 'NONE',  ( -19.74163224554151697, 8.726897413558679872, -232.6665747339030190 ) ) ;
#2266 = CARTESIAN_POINT ( 'NONE',  ( 18.79106389458910442, -5.302521403133691358, -233.5021979784848440 ) ) ;
#2267 = EDGE_CURVE ( 'NONE', #4321, #7303, #16977, .T. ) ;
#2268 = CARTESIAN_POINT ( 'NONE',  ( 4.555016420009541989, 17.65848956729471197, -229.5875910199184204 ) ) ;
#2269 = CARTESIAN_POINT ( 'NONE',  ( -12.87285471141929172, 9.485162256560764504, -229.1865421006261840 ) ) ;
#2270 = CARTESIAN_POINT ( 'NONE',  ( 14.85123888640019452, 5.067529763532427012, -221.9058491819374979 ) ) ;
#2271 = CARTESIAN_POINT ( 'NONE',  ( -12.33332453308451804, -15.34461866416700282, -218.5928953102074388 ) ) ;
#2272 = CARTESIAN_POINT ( 'NONE',  ( 11.21112214669106777, 5.418350954422431975, -227.6539796508718325 ) ) ;
#2273 = VECTOR ( 'NONE', #17556, 1000.000000000000000 ) ;
#2274 = TOROIDAL_SURFACE ( 'NONE', #3700, 10.76794919243112325, 2.000000000000000000 ) ;
#2275 = CARTESIAN_POINT ( 'NONE',  ( 26.00000000000000000, -4.400000000000000355, -3.299999999999998934 ) ) ;
#2276 = CARTESIAN_POINT ( 'NONE',  ( 1.145088139557171036, -28.55736460288477119, -218.6379321102267284 ) ) ;
#2277 = CARTESIAN_POINT ( 'NONE',  ( -7.965409144353247761, 13.56739834143082213, -221.6246244520798712 ) ) ;
#2278 = CARTESIAN_POINT ( 'NONE',  ( 11.64932556965463561, 7.668732705389711413, -229.0406978839571366 ) ) ;
#2279 = CARTESIAN_POINT ( 'NONE',  ( -19.33106196848021341, 9.919700385716687663, -219.0532654734256255 ) ) ;
#2280 = CARTESIAN_POINT ( 'NONE',  ( -12.39195900010699702, 23.13258866008456138, -233.4668451572263166 ) ) ;
#2281 = CARTESIAN_POINT ( 'NONE',  ( 25.70381634773192658, 10.55338509461953400, -230.3576492130207782 ) ) ;
#2282 = CARTESIAN_POINT ( 'NONE',  ( 10.85023464552735462, -16.86364573545779777, -230.5238403791007045 ) ) ;
#2283 = CARTESIAN_POINT ( 'NONE',  ( 19.66153801111809685, -22.47763448259700780, -224.4992982350615023 ) ) ;
#2284 = CARTESIAN_POINT ( 'NONE',  ( 0.9458336400950161371, 17.49535648476021876, -228.8359568483051589 ) ) ;
#2285 = ORIENTED_EDGE ( 'NONE', *, *, #5420, .T. ) ;
#2286 = CARTESIAN_POINT ( 'NONE',  ( 0.000000000000000000, 0.000000000000000000, -103.0000000000000000 ) ) ;
#2287 = CARTESIAN_POINT ( 'NONE',  ( 22.03647168420945590, 0.3315607655625663064, -232.0572713672586644 ) ) ;
#2288 = CARTESIAN_POINT ( 'NONE',  ( -30.16187987321119834, 0.7031948255570967810, -222.4584828387981474 ) ) ;
#2289 = CARTESIAN_POINT ( 'NONE',  ( -8.878187501988019648, -11.23476449186280846, -221.0271673637577123 ) ) ;
#2290 = AXIS2_PLACEMENT_3D ( 'NONE', #7537, #2559, #2674 ) ;
#2291 = CARTESIAN_POINT ( 'NONE',  ( 0.7326557587344989519, -29.96088689026728602, -229.4725774697800205 ) ) ;
#2292 = CARTESIAN_POINT ( 'NONE',  ( 7.508136856874425114, 24.19512352541684663, -230.0608033085341617 ) ) ;
#2293 = CARTESIAN_POINT ( 'NONE',  ( 24.99999999999999645, 1.371045026358143178E-13, 9.000000000000001776 ) ) ;
#2294 = CARTESIAN_POINT ( 'NONE',  ( -14.99655511003079233, 2.316638599135941945, -232.4215266639120046 ) ) ;
#2295 = AXIS2_PLACEMENT_3D ( 'NONE', #9527, #19416, #4437 ) ;
#2296 = CARTESIAN_POINT ( 'NONE',  ( -3.003186468682855104, 15.63968344752823469, -231.5301608670590667 ) ) ;
#2297 = CARTESIAN_POINT ( 'NONE',  ( 1.820119372073704112, 23.17972341190215246, -230.7270437017659503 ) ) ;
#2298 = ORIENTED_EDGE ( 'NONE', *, *, #5629, .F. ) ;
#2299 = CARTESIAN_POINT ( 'NONE',  ( 2.508382434586714282, 15.09451298870656011, -220.9010239894319625 ) ) ;
#2300 = CARTESIAN_POINT ( 'NONE',  ( -26.87016840655871874, 6.086699737350822481, -222.9228935003981746 ) ) ;
#2301 = CARTESIAN_POINT ( 'NONE',  ( 13.72784977962315267, 2.687686193488206143, -220.8507880271885995 ) ) ;
#2302 = CARTESIAN_POINT ( 'NONE',  ( 9.009845654114897684, -15.13764346805314354, -231.2790349225496129 ) ) ;
#2303 = DIRECTION ( 'NONE',  ( 0.000000000000000000, 0.000000000000000000, -1.000000000000000000 ) ) ;
#2304 = VERTEX_POINT ( 'NONE', #19331 ) ;
#2305 = CARTESIAN_POINT ( 'NONE',  ( 8.329997790135040603, 12.51216704542961899, -228.7022893680961602 ) ) ;
#2306 = CARTESIAN_POINT ( 'NONE',  ( 17.64863983146639015, -7.217312291206318342, -219.9249463058993399 ) ) ;
#2307 = CARTESIAN_POINT ( 'NONE',  ( 17.50000000000000355, 0.000000000000000000, -70.00000000000000000 ) ) ;
#2308 = CARTESIAN_POINT ( 'NONE',  ( 0.04660897052267574947, -31.13860575300111577, -224.7746869833732717 ) ) ;
#2309 = SHAPE_DEFINITION_REPRESENTATION ( #4914, #3834 ) ;
#2310 = CARTESIAN_POINT ( 'NONE',  ( -11.42613629117093765, 28.09170287990588832, -228.7150250545069241 ) ) ;
#2311 = CARTESIAN_POINT ( 'NONE',  ( -8.413706464639300719, 10.92140547936800843, -220.6417935981040728 ) ) ;
#2312 = B_SPLINE_CURVE_WITH_KNOTS ( 'NONE', 3,
 ( #6129, #20177, #6355, #11319, #12896, #11207, #2751, #13227, #9632, #16494, #1183, #18073, #8061, #2645, #8510, #18736, #4887, #22220, #3302, #7036, #20630, #15146, #49, #5217, #12205, #15587, #9968, #3528, #10186, #17055, #17269, #15373, #13677, #1842, #165, #3193, #16827, #1405, #12098, #8615, #21988, #15476, #1517, #10076, #15263, #5324, #16941, #18845, #6811, #13791, #20514, #13907, #6922, #4996, #8720, #3085, #6699, #18953, #20407, #11872, #1633, #6581, #5104, #8277, #10408, #20743, #13451, #20292, #11767, #18631, #11984, #8395, #22113, #13571, #3421, #10300, #17164, #1741, #3860, #10741, #10959, #1957, #17606, #12317, #3970, #2173, #7372, #7585, #19495, #14129, #8836, #2283, #17499, #19170, #8946, #21286, #3747, #12540, #498, #7479, #14241, #17382, #10843, #20851, #9052, #17831, #5553, #16031, #16138, #17718, #9168, #19387, #9278, #15920, #21074, #2066, #5662, #10632, #15812, #605, #20965, #388, #5882, #7257, #14349, #21181, #12433, #5766, #19283, #19059, #710, #12648, #14452, #4082, #2394, #3635, #7148, #10516, #14014, #15702, #279, #5433, #16687, #15008, #11178, #11507, #933, #18375, #19714, #4193, #11288, #18269, #16467, #21847, #11070, #12758, #2938, #1267, #6328, #6214, #13089, #19935, #17939, #12867, #9826, #4633, #18044, #8143, #9381, #4523, #20045, #4406, #19608, #2503, #16355, #2614, #7916, #9495, #19820, #4296, #7811, #14676, #11401, #21510, #16242, #6101, #18159, #2831, #12973, #9713, #2724, #819, #7698, #16573, #14567, #9605, #1044, #21621, #21403, #21736, #5994, #14780, #1154, #8031, #14897, #13201, #1605, #12071, #13764, #22081, #15558, #6670, #20602, #8483, #5189, #10161, #10380, #4741, #18928, #6552, #17140, #22195, #6782, #8692, #13306, #6437, #20487, #1814, #16913, #11847, #18712, #8591, #6894, #5078, #24, #20148, #3503, #20264, #17243, #3392, #8366, #11958, #21959, #11619, #10051, #18606, #18492, #13543, #3052, #3275, #9942, #16802, #10274, #1376, #8252, #15120, #13424, #20378, #4861, #1715, #15452, #11738, #3167, #1488, #15236, #4971, #18820, #17030, #15346, #13652, #15674, #7347, #14101, #10717, #10933, #579, #17472, #5297, #5638, #20825, #254, #12405, #17804, #12622, #2371, #19364, #9253, #3945, #20716, #14213, #1931, #20939, #14322, #8921, #10821, #19468, #21048, #12514, #472, #4058, #5526, #21155, #3836, #138, #12178, #5743, #7122, #17691, #2149, #7006, #19256, #15893, #19032, #13988, #13878, #3610, #5405, #10488, #17354, #2260, #7454, #16004, #8811, #12289, #19141, #3721, #9142, #2043, #10603, #15787, #366, #7233, #17583, #9029, #18020, #11047, #9582, #8003, #21484, #9471 ),
 .UNSPECIFIED., .F., .F.,
 ( 4, 2, 2, 2, 2, 2, 2, 2, 2, 2, 2, 2, 2, 2, 2, 2, 2, 2, 2, 2, 2, 2, 2, 2, 2, 2, 2, 2, 2, 2, 2, 2, 2, 2, 2, 2, 2, 2, 2, 2, 2, 2, 2, 2, 2, 2, 2, 2, 2, 2, 2, 2, 2, 2, 2, 2, 2, 2, 2, 2, 2, 2, 2, 2, 2, 2, 2, 2, 2, 2, 2, 2, 2, 2, 2, 2, 2, 2, 2, 2, 2, 2, 2, 2, 2, 2, 2, 2, 2, 2, 2, 2, 2, 2, 2, 2, 2, 2, 2, 2, 2, 2, 2, 2, 2, 2, 2, 2, 2, 2, 2, 2, 2, 2, 2, 2, 2, 2, 2, 2, 2, 2, 2, 2, 2, 2, 2, 2, 2, 2, 2, 2, 2, 2, 2, 2, 2, 2, 2, 2, 2, 2, 2, 2, 2, 2, 2, 2, 2, 2, 2, 2, 2, 2, 2, 2, 2, 2, 2, 2, 2, 2, 2, 2, 2, 2, 2, 2, 2, 4 ),
 ( 0.4999446919652688059, 0.5028747035357847839, 0.5058047151063008728, 0.5087347266768169618, 0.5116647382473329397, 0.5145947498178489177, 0.5175247613883648956, 0.5204547729588808735, 0.5233847845293969625, 0.5268031313616656774, 0.5285123047777999794, 0.5302214781939342814, 0.5336398250262029963, 0.5353489984423374093, 0.5370581718584717112, 0.5404765186907403152, 0.5438948655230090301, 0.5473132123552777450, 0.5507315591875463490, 0.5541499060198149529, 0.5575682528520836678, 0.5609865996843523828, 0.5644049465166209867, 0.5661141199327552886, 0.5678232933488895906, 0.5712416401811581945, 0.5729508135972924965, 0.5746599870134267984, 0.5780783338456955134, 0.5814966806779642283, 0.5849150275102328322, 0.5883333743425015472, 0.5917517211747702621, 0.5951700680070388660, 0.5985884148393075810, 0.6020067616715762959, 0.6037159350877105979, 0.6054251085038448998, 0.6088434553361135038, 0.6122618021683822187, 0.6139709755845166317, 0.6156801490006509336, 0.6190984958329195376, 0.6225168426651882525, 0.6259351894974569674, 0.6293535363297255714, 0.6327718831619942863, 0.6361902299942630012, 0.6396085768265316052, 0.6430269236588003201, 0.6447360970749347331, 0.6464452704910690350, 0.6498636173233376390, 0.6532819641556063539, 0.6549911375717407669, 0.6567003109878750688, 0.6601186578201436728, 0.6635370046524122767, 0.6669553514846809916, 0.6703736983169497066, 0.6737920451492183105, 0.6772103919814870254, 0.6806287388137557404, 0.6840470856460243443, 0.6857562590621586462, 0.6866108457702257972, 0.6874654324782930592, 0.6908837793105617742, 0.6943021261428303781, 0.6960112995589646800, 0.6977204729750989820, 0.7011388198073676969, 0.7045571666396364119, 0.7079755134719050158, 0.7113938603041736197, 0.7148122071364423347, 0.7182305539687110496, 0.7216489008009796535, 0.7250672476332483685, 0.7267764210493827814, 0.7284855944655170834, 0.7319039412977856873, 0.7353222881300544023, 0.7387406349623231172, 0.7421589817945917211, 0.7455773286268603250, 0.7489956754591290400, 0.7524140222913977549, 0.7558323691236663588, 0.7592507159559350738, 0.7626690627882037887, 0.7660874096204723926, 0.7695057564527411076, 0.7729241032850098225, 0.7763424501172784264, 0.7797607969495471414, 0.7831791437818158563, 0.7865974906140844602, 0.7900158374463531752, 0.7934341842786218901, 0.7968525311108904940, 0.8002708779431590980, 0.8036892247754278129, 0.8053983981915622259, 0.8071075716076965278, 0.8105259184399651318, 0.8122350918560994337, 0.8139442652722337357, 0.8173626121045024506, 0.8207809589367711656, 0.8241993057690397695, 0.8276176526013083734, 0.8310359994335770883, 0.8344543462658458033, 0.8378726930981144072, 0.8412910399303831221, 0.8430002133465175351, 0.8447093867626518371, 0.8481277335949204410, 0.8515460804271891559, 0.8549644272594578709, 0.8583827740917264748, 0.8618011209239951897, 0.8652194677562639047, 0.8686378145885325086, 0.8720561614208012235, 0.8754745082530699385, 0.8788928550853385424, 0.8823112019176071463, 0.8857295487498758613, 0.8874387221660102743, 0.8891478955821445762, 0.8925662424144131801, 0.8942754158305474821, 0.8959845892466818951, 0.8994029360789506100, 0.9028212829112192139, 0.9062396297434879289, 0.9096579765757566438, 0.9130763234080252477, 0.9164946702402939627, 0.9199130170725626776, 0.9233313639048312815, 0.9250405373209655835, 0.9267497107370999965, 0.9301680575693687114, 0.9335864044016373153, 0.9352955778177716173, 0.9370047512339059192, 0.9404230980661746342, 0.9438414448984433491, 0.9472597917307119531, 0.9506781385629806680, 0.9540964853952493829, 0.9575148322275179869, 0.9609331790597867018, 0.9643515258920554167, 0.9660606993081897187, 0.9677698727243240207, 0.9711882195565927356, 0.9728973929727271486, 0.9746065663888614505, 0.9780249132211300545, 0.9814432600533987694, 0.9848616068856674843, 0.9882799537179360883, 0.9912099652884520662, 0.9941399768589680441, 0.9970699884294840221, 1.000000000000000000 ),
 .UNSPECIFIED. ) ;
#2313 = CARTESIAN_POINT ( 'NONE',  ( -8.172572110426221670, 16.86653848210977813, -233.4220330256369493 ) ) ;
#2314 = CARTESIAN_POINT ( 'NONE',  ( -14.03072379416114757, -18.13329758221107824, -232.5220584501505812 ) ) ;
#2315 = CARTESIAN_POINT ( 'NONE',  ( 0.000000000000000000, 0.000000000000000000, -77.51594804401857175 ) ) ;
#2316 = DIRECTION ( 'NONE',  ( -1.000000000000000000, 0.000000000000000000, 0.000000000000000000 ) ) ;
#2317 = CARTESIAN_POINT ( 'NONE',  ( -7.429838964355703901, 14.87322129099639234, -232.2632863647814077 ) ) ;
#2318 = CARTESIAN_POINT ( 'NONE',  ( 3.810076078852552950, -13.18001539772800612, -226.2402971015400510 ) ) ;
#2319 = CARTESIAN_POINT ( 'NONE',  ( 0.000000000000000000, 0.000000000000000000, -24.99999999999999645 ) ) ;
#2320 = CARTESIAN_POINT ( 'NONE',  ( -21.02719846458807851, 18.12262440796364871, -218.0220709499931502 ) ) ;
#2321 = EDGE_CURVE ( 'NONE', #19351, #20853, #6917, .T. ) ;
#2322 = CARTESIAN_POINT ( 'NONE',  ( 13.80707869872719762, 6.429545566348308760, -225.7152177910682553 ) ) ;
#2323 = CARTESIAN_POINT ( 'NONE',  ( -23.95129667199961077, 20.99391807043993552, -227.1541646794576081 ) ) ;
#2324 = CARTESIAN_POINT ( 'NONE',  ( 0.000000000000000000, 0.000000000000000000, -75.00000000000000000 ) ) ;
#2325 = CARTESIAN_POINT ( 'NONE',  ( 16.01130065545721592, 20.79417322911648114, -220.9619135886794652 ) ) ;
#2326 = CARTESIAN_POINT ( 'NONE',  ( -7.589660848220153078, -14.86992855705293692, -228.0480809167547136 ) ) ;
#2327 = ORIENTED_EDGE ( 'NONE', *, *, #9143, .F. ) ;
#2328 = CARTESIAN_POINT ( 'NONE',  ( -3.223980134944351317, 26.83284996841001302, -219.5167893230652965 ) ) ;
#2329 = CARTESIAN_POINT ( 'NONE',  ( -12.80756961294691010, 26.82110654133967387, -223.7464923486294026 ) ) ;
#2330 = CARTESIAN_POINT ( 'NONE',  ( -18.17591565587962776, 16.23604867791855355, -233.2845329962925121 ) ) ;
#2331 = CIRCLE ( 'NONE', #18866, 9.000000000000001776 ) ;
#2332 = CARTESIAN_POINT ( 'NONE',  ( -16.14140970932308505, -18.57031478189210816, -230.2506069696216287 ) ) ;
#2333 = DIRECTION ( 'NONE',  ( 1.000000000000000000, 0.000000000000000000, 0.000000000000000000 ) ) ;
#2334 = VERTEX_POINT ( 'NONE', #8774 ) ;
#2335 = COLOUR_RGB ( '', 0.72549020, 0.75294118, 0.79215686) ;
#2336 = CARTESIAN_POINT ( 'NONE',  ( -14.10849459794400751, -0.2436790717799666162, -223.1085195285415921 ) ) ;
#2337 = CARTESIAN_POINT ( 'NONE',  ( 7.240923751923983964, -14.90955521745277501, -222.5312387745455283 ) ) ;
#2338 = CARTESIAN_POINT ( 'NONE',  ( 14.85123888640019452, 5.067529763532427012, -221.9058491819374979 ) ) ;
#2339 = CARTESIAN_POINT ( 'NONE',  ( -0.3969026096611234511, 20.89748314411456676, -216.3289738411752978 ) ) ;
#2340 = CARTESIAN_POINT ( 'NONE',  ( 18.50073117969547098, -1.889592114545683987, -232.6396648696776026 ) ) ;
#2341 = CARTESIAN_POINT ( 'NONE',  ( 11.78717493688862206, 28.63884142527983556, -229.7724827508652652 ) ) ;
#2342 = CARTESIAN_POINT ( 'NONE',  ( 10.83706092800007781, 10.12544885278926543, -227.1716144446442343 ) ) ;
#2343 = DIRECTION ( 'NONE',  ( -1.000000000000000000, 0.000000000000000000, 0.000000000000000000 ) ) ;
#2344 = VECTOR ( 'NONE', #17003, 1000.000000000000000 ) ;
#2345 = CARTESIAN_POINT ( 'NONE',  ( -12.42894476027428929, -17.97759322220185396, -216.3110355466728834 ) ) ;
#2346 = AXIS2_PLACEMENT_3D ( 'NONE', #19041, #4979, #6679 ) ;
#2347 = CARTESIAN_POINT ( 'NONE',  ( 8.021672912688133650, -23.92397517040199872, -233.3380040120402441 ) ) ;
#2348 = CARTESIAN_POINT ( 'NONE',  ( 0.000000000000000000, 0.000000000000000000, -60.00000000000000000 ) ) ;
#2349 = DIRECTION ( 'NONE',  ( 0.000000000000000000, 0.000000000000000000, -1.000000000000000000 ) ) ;
#2350 = CARTESIAN_POINT ( 'NONE',  ( -11.80036766549451599, 3.629178540272184783, -221.4826559383200220 ) ) ;
#2351 = CARTESIAN_POINT ( 'NONE',  ( -19.94082127283490280, -7.534429669270808816, -230.8553971038493557 ) ) ;
#2352 = CARTESIAN_POINT ( 'NONE',  ( -17.49393085256189906, 10.63366922396483361, -217.7502683347138657 ) ) ;
#2353 = CARTESIAN_POINT ( 'NONE',  ( 23.22505041959077232, 19.39625294115234055, -221.5972645870541555 ) ) ;
#2354 = CARTESIAN_POINT ( 'NONE',  ( 17.35243190875273811, 16.67741344734974263, -230.5744436858935558 ) ) ;
#2355 = VERTEX_POINT ( 'NONE', #5486 ) ;
#2356 = CARTESIAN_POINT ( 'NONE',  ( 7.445043070300236820, -12.68569377707410339, -219.2962123921901991 ) ) ;
#2357 = CARTESIAN_POINT ( 'NONE',  ( 12.71450444683213021, 7.595266944807587350, -224.4213778964231665 ) ) ;
#2358 = EDGE_CURVE ( 'NONE', #20525, #20136, #5458, .T. ) ;
#2359 = CARTESIAN_POINT ( 'NONE',  ( -4.695076324262313250, 31.85502299853856201, -223.8918597786031341 ) ) ;
#2360 = CARTESIAN_POINT ( 'NONE',  ( -4.365576370787875859, 13.02741211227440665, -230.2897948137907917 ) ) ;
#2361 = CARTESIAN_POINT ( 'NONE',  ( -28.12632608809566293, -1.403418003803144742, -218.5233027210585988 ) ) ;
#2362 = CARTESIAN_POINT ( 'NONE',  ( -25.80904414196669450, 12.19501778665756220, -219.1732313092283846 ) ) ;
#2363 = PLANE ( 'NONE',  #18045 ) ;
#2364 = CIRCLE ( 'NONE', #7779, 25.52219491023488018 ) ;
#2365 = VECTOR ( 'NONE', #21604, 1000.000000000000000 ) ;
#2366 = CARTESIAN_POINT ( 'NONE',  ( 27.32546652195855685, -7.354568365469916991, -229.0866163655393279 ) ) ;
#2367 = CARTESIAN_POINT ( 'NONE',  ( 1.984991703947643904, 14.51738422979996912, -218.4500278854917781 ) ) ;
#2368 = CARTESIAN_POINT ( 'NONE',  ( 14.81251837262747983, -1.020578734748967209, -221.0290343291311785 ) ) ;
#2369 = CARTESIAN_POINT ( 'NONE',  ( 15.70515172005171323, -0.7403987186381333352, -226.4590404369862995 ) ) ;
#2370 = CARTESIAN_POINT ( 'NONE',  ( 4.543450689403089271, 15.91052110650461771, -218.9437823786444426 ) ) ;
#2371 = CARTESIAN_POINT ( 'NONE',  ( -16.38803511840525218, -9.809678413005567421, -217.1940421839195494 ) ) ;
#2372 = CARTESIAN_POINT ( 'NONE',  ( -2.043230952238195286, 23.63069326910348877, -232.6835180461029040 ) ) ;
#2373 = CARTESIAN_POINT ( 'NONE',  ( -1.608171596096409806, -16.77465153034988887, -217.4618546331240054 ) ) ;
#2374 = CARTESIAN_POINT ( 'NONE',  ( 13.61707622192329481, 14.84143455326118932, -217.6958999636067063 ) ) ;
#2375 = CARTESIAN_POINT ( 'NONE',  ( 20.24215890739238688, -18.92204689856563249, -233.5548650425709241 ) ) ;
#2376 = DIRECTION ( 'NONE',  ( 1.000000000000000000, 0.000000000000000000, 0.000000000000000000 ) ) ;
#2377 = CARTESIAN_POINT ( 'NONE',  ( -12.43544732248594720, 12.69828336922617318, -219.3367909706387877 ) ) ;
#2378 = DIRECTION ( 'NONE',  ( -0.000000000000000000, 0.000000000000000000, -1.000000000000000000 ) ) ;
#2379 = CARTESIAN_POINT ( 'NONE',  ( -26.22128172021140813, -2.843310382428120064, -218.3980250098940132 ) ) ;
#2380 = CARTESIAN_POINT ( 'NONE',  ( 6.608541902967795423, 16.43938546752961116, -220.2982508316308952 ) ) ;
#2381 = CARTESIAN_POINT ( 'NONE',  ( -16.28025842329327944, 6.985656672962045732, -231.4191468057695715 ) ) ;
#2382 = CARTESIAN_POINT ( 'NONE',  ( 25.80927844399814930, 11.21489550116160316, -221.3538377621514996 ) ) ;
#2383 = CARTESIAN_POINT ( 'NONE',  ( -7.215839073791710412, -12.32959168003491968, -224.1142876912989834 ) ) ;
#2384 = CARTESIAN_POINT ( 'NONE',  ( 17.85905871012913693, 8.463974683125162102, -234.6532732619751300 ) ) ;
#2385 = CARTESIAN_POINT ( 'NONE',  ( -10.53630953054794794, -7.637555647514923329, -229.7964863767589918 ) ) ;
#2386 = CARTESIAN_POINT ( 'NONE',  ( 5.955271202636533090, 21.50135983300913267, -233.0184468368920534 ) ) ;
#2387 = CARTESIAN_POINT ( 'NONE',  ( 27.79746884017060538, 13.63637251724950339, -226.5788410723774575 ) ) ;
#2388 = CARTESIAN_POINT ( 'NONE',  ( -9.852301241816233457, 15.10013604187968461, -230.8124578431014697 ) ) ;
#2389 = EDGE_CURVE ( 'NONE', #18055, #3468, #17936, .T. ) ;
#2390 = CARTESIAN_POINT ( 'NONE',  ( -3.687581766460184429, 30.01855770642711718, -218.8323691868875187 ) ) ;
#2391 = CARTESIAN_POINT ( 'NONE',  ( -20.26851768784797869, -0.8260594303982465858, -217.1279713726092098 ) ) ;
#2392 = ORIENTED_EDGE ( 'NONE', *, *, #13238, .F. ) ;
#2393 = CARTESIAN_POINT ( 'NONE',  ( 0.3833872033527188639, -14.95856321834011915, -223.3240416624371107 ) ) ;
#2394 = CARTESIAN_POINT ( 'NONE',  ( 4.823266655078461085, -13.86048651889774241, -224.7145696108100026 ) ) ;
#2395 = EDGE_CURVE ( 'NONE', #21209, #22159, #3546, .T. ) ;
#2396 = CARTESIAN_POINT ( 'NONE',  ( 0.000000000000000000, 20.99999999999999645, -69.99999999999998579 ) ) ;
#2397 = CARTESIAN_POINT ( 'NONE',  ( 14.54149994592679107, 8.070685273005897997, -229.7292930672863349 ) ) ;
#2398 = CARTESIAN_POINT ( 'NONE',  ( -13.36635042947306573, -0.3940246778032021058, -227.3384152261055249 ) ) ;
#2399 = EDGE_CURVE ( 'NONE', #7331, #8832, #5603, .T. ) ;
#2400 = CARTESIAN_POINT ( 'NONE',  ( -17.58118739749173898, -8.238107657346720458, -217.5252134542318458 ) ) ;
#2401 = CARTESIAN_POINT ( 'NONE',  ( 8.257114973007913861, -25.39836461225790742, -232.6217252414676295 ) ) ;
#2402 = CARTESIAN_POINT ( 'NONE',  ( 12.83388873239664996, 22.07510045760132655, -230.4740059944613222 ) ) ;
#2403 = FACE_OUTER_BOUND ( 'NONE', #7697, .T. ) ;
#2404 = CARTESIAN_POINT ( 'NONE',  ( -12.88152464663890306, 6.317716727793897924, -230.5294309895745073 ) ) ;
#2405 = CARTESIAN_POINT ( 'NONE',  ( -7.429838964355703901, 14.87322129099639234, -232.2632863647814077 ) ) ;
#2406 = CARTESIAN_POINT ( 'NONE',  ( 3.325336547283623378, 18.92213121405483633, -219.7480163085221818 ) ) ;
#2407 = CARTESIAN_POINT ( 'NONE',  ( 24.67321061357916889, 1.914345543126667826, -232.4367140101115581 ) ) ;
#2408 = ORIENTED_EDGE ( 'NONE', *, *, #21324, .T. ) ;
#2409 = CARTESIAN_POINT ( 'NONE',  ( 11.09231067055629616, 7.417581979752235100, -227.5152062457793534 ) ) ;
#2410 = CARTESIAN_POINT ( 'NONE',  ( -15.95412330064426065, 13.09400588185824077, -218.6613039563597169 ) ) ;
#2411 = CARTESIAN_POINT ( 'NONE',  ( 14.96462366732929716, 7.179279272144128754, -233.2042342402542374 ) ) ;
#2412 = CARTESIAN_POINT ( 'NONE',  ( -7.180402128846711918, -26.42159752827261698, -220.2116303544826224 ) ) ;
#2413 = DIRECTION ( 'NONE',  ( 0.000000000000000000, 1.000000000000000000, -0.000000000000000000 ) ) ;
#2414 = EDGE_LOOP ( 'NONE', ( #22124, #8855 ) ) ;
#2415 = CARTESIAN_POINT ( 'NONE',  ( 3.763426558366607111, 28.60172112197566818, -230.1816715025297526 ) ) ;
#2416 = CARTESIAN_POINT ( 'NONE',  ( 15.78601976571614962, -10.64697985159532401, -219.7411765650222151 ) ) ;
#2417 = CARTESIAN_POINT ( 'NONE',  ( -22.10934047915427314, 0.9940043559354312386, -216.9999999999999716 ) ) ;
#2418 = CARTESIAN_POINT ( 'NONE',  ( 7.958080982411646076, -16.12895853103474408, -217.0903302464454612 ) ) ;
#2419 = APPLICATION_PROTOCOL_DEFINITION ( 'draft international standard', 'automotive_design', 1998, #12889 ) ;
#2420 = CARTESIAN_POINT ( 'NONE',  ( -1.249406995060579062, 25.48934319316224162, -216.9406480707515072 ) ) ;
#2421 = CARTESIAN_POINT ( 'NONE',  ( -11.10182655035041144, 8.778638955377752850, -227.1050196202568827 ) ) ;
#2422 = ORIENTED_EDGE ( 'NONE', *, *, #6882, .F. ) ;
#2423 = CARTESIAN_POINT ( 'NONE',  ( -17.65835845419170624, 22.55329142274348442, -231.2673511165784532 ) ) ;
#2424 = CARTESIAN_POINT ( 'NONE',  ( -14.26331330459994540, -11.99770975811722451, -232.1846756268951708 ) ) ;
#2425 = DIRECTION ( 'NONE',  ( 0.000000000000000000, 0.000000000000000000, 1.000000000000000000 ) ) ;
#2426 = DIRECTION ( 'NONE',  ( 1.000000000000000000, -0.000000000000000000, -0.000000000000000000 ) ) ;
#2427 = CARTESIAN_POINT ( 'NONE',  ( -3.501680520304516264, 14.31538576447642264, -219.8967178229432307 ) ) ;
#2428 = CARTESIAN_POINT ( 'NONE',  ( 1.145088139557171036, -28.55736460288477119, -218.6379321102267284 ) ) ;
#2429 = CARTESIAN_POINT ( 'NONE',  ( 14.21523762536935820, -1.512798260419094598, -222.4093369397272397 ) ) ;
#2430 = CARTESIAN_POINT ( 'NONE',  ( -14.00380962569832199, 8.747390586476997854, -231.7950903513155936 ) ) ;
#2431 = CARTESIAN_POINT ( 'NONE',  ( -19.26845014167239611, 9.481468541508135672, -234.4856117705182328 ) ) ;
#2432 = CARTESIAN_POINT ( 'NONE',  ( -9.060295054034883222, 29.20313342278041802, -224.2979742714222482 ) ) ;
#2433 = CARTESIAN_POINT ( 'NONE',  ( 0.000000000000000000, 0.000000000000000000, -60.00000000000000000 ) ) ;
#2434 = CARTESIAN_POINT ( 'NONE',  ( 21.15841376125116824, 4.865517895153391947, -217.1795922978051578 ) ) ;
#2435 = CARTESIAN_POINT ( 'NONE',  ( -6.842387616420496421, -14.58019248909694632, -223.2484495378617453 ) ) ;
#2436 = VERTEX_POINT ( 'NONE', #8887 ) ;
#2437 = CARTESIAN_POINT ( 'NONE',  ( 5.955271202636533090, 21.50135983300913267, -233.0184468368920534 ) ) ;
#2438 = CARTESIAN_POINT ( 'NONE',  ( -14.22959263369750182, 18.28478771081826793, -217.8090497856120464 ) ) ;
#2439 = CARTESIAN_POINT ( 'NONE',  ( -9.403561938624596550, 12.70246821120386471, -220.7484614495429582 ) ) ;
#2440 = ORIENTED_EDGE ( 'NONE', *, *, #14341, .F. ) ;
#2441 = CARTESIAN_POINT ( 'NONE',  ( 28.19769730429874599, -1.268543021275377658, -231.5188709829604363 ) ) ;
#2442 = CARTESIAN_POINT ( 'NONE',  ( 0.000000000000000000, 21.80000000000000071, -78.50000000000000000 ) ) ;
#2443 = ORIENTED_EDGE ( 'NONE', *, *, #14102, .F. ) ;
#2444 = CARTESIAN_POINT ( 'NONE',  ( -13.69675006931110417, 3.702342960760605539, -228.0723273272095355 ) ) ;
#2445 = CARTESIAN_POINT ( 'NONE',  ( 7.487558183825500535, -19.68056729374139380, -230.9679144533258466 ) ) ;
#2446 = CARTESIAN_POINT ( 'NONE',  ( 14.32085100525799248, 9.220655089380342062, -219.9006227404039464 ) ) ;
#2447 = CARTESIAN_POINT ( 'NONE',  ( -3.755296588130283553, 23.77975947300719284, -233.7323173085780752 ) ) ;
#2448 = DIRECTION ( 'NONE',  ( -1.000000000000000000, 0.000000000000000000, -0.000000000000000000 ) ) ;
#2449 = CARTESIAN_POINT ( 'NONE',  ( -16.90857133559978465, -0.4126725064255206687, -221.6276144895144569 ) ) ;
#2450 = CARTESIAN_POINT ( 'NONE',  ( 7.803634760976553508, 10.78293796201124266, -229.6314106675118865 ) ) ;
#2451 = CARTESIAN_POINT ( 'NONE',  ( 12.99034161053428349, 11.71468708507361889, -230.9043293568357740 ) ) ;
#2452 = AXIS2_PLACEMENT_3D ( 'NONE', #1975, #17738, #14032 ) ;
#2453 = DIRECTION ( 'NONE',  ( 1.000000000000000000, 0.000000000000000000, 0.000000000000000000 ) ) ;
#2454 = CARTESIAN_POINT ( 'NONE',  ( -6.870552667427666904, -18.85419487977974029, -216.2130481585807047 ) ) ;
#2455 = CARTESIAN_POINT ( 'NONE',  ( 15.10937218716165020, -26.44221868192832758, -222.7999243300199907 ) ) ;
#2456 = DIRECTION ( 'NONE',  ( 0.000000000000000000, 0.000000000000000000, -1.000000000000000000 ) ) ;
#2457 = CARTESIAN_POINT ( 'NONE',  ( 0.000000000000000000, 23.00000000000006040, 75.00000000000000000 ) ) ;
#2458 = CARTESIAN_POINT ( 'NONE',  ( -8.328662059352005542, 28.53523473722178139, -221.4280032538016201 ) ) ;
#2459 = CARTESIAN_POINT ( 'NONE',  ( 14.54962894845190036, -2.357901078066860112, -232.0046840244626765 ) ) ;
#2460 = CARTESIAN_POINT ( 'NONE',  ( 27.96460686140487084, -1.872811165202790340, -220.9791906660856000 ) ) ;
#2461 = CARTESIAN_POINT ( 'NONE',  ( 19.40629804599390340, 15.10110417999774057, -216.3942729496570223 ) ) ;
#2462 = CARTESIAN_POINT ( 'NONE',  ( 11.40028598017942230, 13.60807601628675023, -220.9105305289655519 ) ) ;
#2463 = ORIENTED_EDGE ( 'NONE', *, *, #3719, .F. ) ;
#2464 = CARTESIAN_POINT ( 'NONE',  ( 22.27668549480667792, -16.40903445915953895, -216.4638184065479152 ) ) ;
#2465 = CARTESIAN_POINT ( 'NONE',  ( 10.60004861036625812, 9.899508790423018567, 93.00000000000001421 ) ) ;
#2466 = EDGE_CURVE ( 'NONE', #14946, #18185, #13256, .T. ) ;
#2467 = CARTESIAN_POINT ( 'NONE',  ( -2.218529449563984901, 24.06491599887877442, -214.8915873797660652 ) ) ;
#2468 = CARTESIAN_POINT ( 'NONE',  ( -5.543543819386913540, 14.51457927969963713, -217.3847528063896846 ) ) ;
#2469 = CARTESIAN_POINT ( 'NONE',  ( -12.65123680455331190, -6.798726433138870817, -228.2089845657881710 ) ) ;
#2470 = CARTESIAN_POINT ( 'NONE',  ( -18.70100282803782576, 16.58357028540773115, -216.4425743468854080 ) ) ;
#2471 = AXIS2_PLACEMENT_3D ( 'NONE', #3911, #10565, #10684 ) ;
#2472 = CARTESIAN_POINT ( 'NONE',  ( 0.000000000000000000, 0.000000000000000000, 75.00000000000000000 ) ) ;
#2473 = CARTESIAN_POINT ( 'NONE',  ( 18.22947608839760747, -6.525328669204546905, -217.7409786913911205 ) ) ;
#2474 = CARTESIAN_POINT ( 'NONE',  ( -1.406618399933933006, 16.47239985789244443, -232.2564017133012726 ) ) ;
#2475 = CARTESIAN_POINT ( 'NONE',  ( 20.92846067405557520, -2.114533307883533109, -233.2756072794335580 ) ) ;
#2476 = CARTESIAN_POINT ( 'NONE',  ( -11.49049084071896409, 11.06834963248926940, -218.3354249205727058 ) ) ;
#2477 = CARTESIAN_POINT ( 'NONE',  ( 15.33737796850231305, 13.57479350230705428, -232.3313557812109025 ) ) ;
#2478 = DIRECTION ( 'NONE',  ( 0.000000000000000000, 0.000000000000000000, -1.000000000000000000 ) ) ;
#2479 = CARTESIAN_POINT ( 'NONE',  ( 5.142103055192286831, 28.18228231877369439, -225.8998064704803994 ) ) ;
#2480 = CARTESIAN_POINT ( 'NONE',  ( -16.21268175593173311, -5.852138355245464219, -231.1837890105803410 ) ) ;
#2482 = B_SPLINE_CURVE_WITH_KNOTS ( 'NONE', 3,
 ( #2417, #2636, #11093, #2744, #956, #14695, #12671, #13109, #7719, #9299, #16486, #19519, #17960, #4105, #10983, #14590, #12992, #1063, #7936, #21425, #21308, #14800, #21642, #6236, #2849, #4762, #1733, #3411, #20397, #4988, #6689, #22211, #1396, #18396, #13220, #9960, #15255, #13563, #6457, #3184, #9847, #8500, #18837, #10068, #10291, #1507, #21978, #8162, #16932, #6572, #11863, #16708, #3072, #3293, #8607, #11639, #13326, #18510, #17157, #11976, #20504, #5095, #18623, #8387, #15467, #6348, #20168, #20065, #4653, #15365, #18728, #2961, #10178, #8270, #1288, #13443, #15137, #22101, #11526, #15028, #17047, #16819, #21867, #20283, #1623, #4878, #11757, #6801, #13669, #17490, #20956, #21067, #3961, #17709, #12088, #14232, #3626, #5205, #19161, #5544, #7364, #3737, #3519, #12195, #10399, #10621, #18944, #20622, #12532, #19051, #269, #17259, #10836, #5313, #2277, #2058, #491, #10505, #1831, #8709, #9160, #381, #12306, #15576, #41, #6912, #20733, #5655, #17372, #19380, #7024, #13783, #8936, #1947, #155, #12423, #13896, #8826, #15691, #7139, #15803, #14005, #19274, #20841, #5424, #7249, #14120, #3853, #10733, #17598, #2165, #9045, #15911, #21503, #11394, #9375, #19600, #5872, #924, #7692, #16235, #2826, #4187, #6093, #11063, #17933, #2495, #17824, #12862, #811, #7804, #19486, #12752, #12968, #18262, #21279, #16129, #14560, #13083, #21614, #7911, #16022, #21172, #21396, #9271, #14669, #5988, #4291, #4514, #16462, #19706, #5759, #19813, #19928, #14444, #7470, #597, #702, #9488, #11170, #4397, #18038, #2386, #2606, #12639, #7578, #4076, #16350, #14339, #10951, #11282, #18152, #2717, #9599, #1037, #14774, #6205, #13300, #18598, #16906, #9817, #1370, #20481, #11841, #10154, #20256, #20141, #9933, #14888, #8359, #8022, #4964, #1482, #5072, #16795, #4734, #15340, #11950, #6776, #6431, #17022, #4853, #16680, #8246, #6664, #11730, #22188, #1598, #3046, #18813, #15114, #8477, #4626, #16566, #21951, #1146, #21729, #13645, #1260, #20372, #13535, #11611, #18483, #6320, #9706, #15229, #13194, #6544, #13415, #3161, #18706, #20039, #11500, #2930, #10045, #3269, #8135, #18369, #15001, #22074, #21839, #18922, #465, #6999, #15551, #10712, #10481, #17237, #1924, #20595, #15447, #2144, #10374, #17134, #5398, #1808, #3497, #8915, #1709, #5634, #9024, #14094, #7228, #8685, #15782, #17, #8584, #130, #15886, #17577, #13872, #7341, #6887, #19134, #13757, #360, #21044, #19027, #20711, #5292, #10596, #12172, #14208, #12510, #3604, #20933, #17346, #8805 ),
 .UNSPECIFIED., .F., .F.,
 ( 4, 2, 2, 2, 2, 2, 2, 2, 2, 2, 2, 2, 2, 2, 2, 2, 2, 2, 2, 2, 2, 2, 2, 2, 2, 2, 2, 2, 2, 2, 2, 2, 2, 2, 2, 2, 2, 2, 2, 2, 2, 2, 2, 2, 2, 2, 2, 2, 2, 2, 2, 2, 2, 2, 2, 2, 2, 2, 2, 2, 2, 2, 2, 2, 2, 2, 2, 2, 2, 2, 2, 2, 2, 2, 2, 2, 2, 2, 2, 2, 2, 2, 2, 2, 2, 2, 2, 2, 2, 2, 2, 2, 2, 2, 2, 2, 2, 2, 2, 2, 2, 2, 2, 2, 2, 2, 2, 2, 2, 2, 2, 2, 2, 2, 2, 2, 2, 2, 2, 2, 2, 2, 2, 2, 2, 2, 2, 2, 2, 2, 2, 2, 2, 2, 2, 2, 2, 2, 2, 2, 2, 2, 2, 2, 2, 2, 2, 2, 2, 2, 2, 2, 2, 2, 2, 2, 2, 2, 2, 2, 2, 2, 2, 4 ),
 ( 0.000000000000000000, 0.001952908952989333875, 0.003905817905978667751, 0.007323408573709997045, 0.01074099924144132634, 0.01415858990917265650, 0.01586738524303832332, 0.01757618057690398666, 0.02099377124463531682, 0.02441136191236664699, 0.02782895258009797368, 0.03124654324782930384, 0.03466413391556063400, 0.03808172458329196070, 0.04149931525102329433, 0.04491690591875462102, 0.04662570125262028436, 0.04833449658648594771, 0.05175208725421727440, 0.05346088258808293775, 0.05516967792194860110, 0.05858726858967993473, 0.06200485925741126836, 0.06542244992514259505, 0.06884004059287393562, 0.07225763126060526231, 0.07567522192833658901, 0.07909281259606792958, 0.08251040326379925627, 0.08421919859766491268, 0.08592799393153058296, 0.08934558459926195129, 0.09276317526699331961, 0.09447197060085900377, 0.09618076593472468794, 0.09959835660245604239, 0.1030159472701873968, 0.1064335379379187652, 0.1098511286056501335, 0.1132687192733815018, 0.1166863099411127869, 0.1201039006088440858, 0.1235214912765753847, 0.1252302866104410273, 0.1269390819443066698, 0.1303566726120379826, 0.1320654679459036251, 0.1337742632797692677, 0.1371918539475005527, 0.1406094446152318378, 0.1440270352829631784, 0.1474446259506944912, 0.1508622166184258040, 0.1542798072861571446, 0.1576973979538884851, 0.1611149886216198257, 0.1645325792893511663, 0.1679501699570824791, 0.1713677606248137919, 0.1747853512925451325, 0.1764941466264108028, 0.1782029419602764730, 0.1816205326280078136, 0.1850381232957391542, 0.1884557139634704670, 0.1918733046312017798, 0.1952908952989331204, 0.1987084859666644610, 0.2021260766343957738, 0.2055436673021270866, 0.2072524626359927569, 0.2089612579698584272, 0.2123788486375897677, 0.2140876439714554380, 0.2157964393053211083, 0.2192140299730524489, 0.2226316206407837617, 0.2260492113085151300, 0.2294668019762464706, 0.2328843926439778111, 0.2363019833117091517, 0.2397195739794404923, 0.2431371646471718329, 0.2465547553149031734, 0.2499723459826345140, 0.2533899366503657991, 0.2568075273180971396, 0.2602251179858284802, 0.2636427086535597653, 0.2670602993212909948, 0.2704778899890223909, 0.2738954806567537315, 0.2773130713244850165, 0.2807306619922163571, 0.2841482526599476977, 0.2858570479938133957, 0.2875658433276790382, 0.2909834339954103788, 0.2926922293292760768, 0.2944010246631417194, 0.2978186153308730599, 0.3012362059986043450, 0.3046537966663356856, 0.3080713873340670261, 0.3114889780017983112, 0.3149065686695296518, 0.3183241593372609923, 0.3217417500049923329, 0.3234505453388579754, 0.3251593406727236735, 0.3285769313404549585, 0.3319945220081862991, 0.3354121126759176397, 0.3388297033436489247, 0.3422472940113802653, 0.3456648846791116059, 0.3490824753468429464, 0.3525000660145742870, 0.3559176566823056276, 0.3593352473500369682, 0.3627528380177683087, 0.3661704286854996493, 0.3695880193532309343, 0.3730056100209622749, 0.3747144053548279174, 0.3764232006886936155, 0.3798407913564249005, 0.3832583820241562411, 0.3866759726918875817, 0.3900935633596189223, 0.3935111540273502628, 0.3969287446950816034, 0.4003463353628129440, 0.4037639260305442845, 0.4054727213644099271, 0.4071815166982756251, 0.4105991073660069102, 0.4140166980337382507, 0.4157254933676038933, 0.4174342887014695913, 0.4208518793692008764, 0.4242694700369322169, 0.4276870607046635575, 0.4311046513723948981, 0.4345222420401262386, 0.4379398327078575237, 0.4413574233755888643, 0.4447750140433202048, 0.4464838093771859029, 0.4481926047110515454, 0.4516101953787828860, 0.4533189907126485840, 0.4550277860465142266, 0.4584453767142455671, 0.4618629673819769077, 0.4652805580497082483, 0.4686981487174395888, 0.4721157393851709294, 0.4755333300529022145, 0.4789509207206334995, 0.4823685113883648956, 0.4840773067222305381, 0.4857861020560961807, 0.4878404479772363023 ),
 .UNSPECIFIED. ) ;
#2481 = CARTESIAN_POINT ( 'NONE',  ( 26.29894631880581812, 12.29609390142961090, -226.3100047295820332 ) ) ;
#2483 = CARTESIAN_POINT ( 'NONE',  ( -0.1874296312810625753, -16.87674362306512776, -233.1597105263269611 ) ) ;
#2484 = CARTESIAN_POINT ( 'NONE',  ( 19.66316721362388975, 2.213178807039652973, -222.9648072419893765 ) ) ;
#2485 = CARTESIAN_POINT ( 'NONE',  ( -13.70798801564395752, 13.71024986321384809, -218.3360451569033955 ) ) ;
#2486 = CARTESIAN_POINT ( 'NONE',  ( -23.00000000000008882, 0.000000000000000000, 75.00000000000000000 ) ) ;
#2487 = CARTESIAN_POINT ( 'NONE',  ( -25.99367553232993799, -4.794975032520305547, -231.0351783075731191 ) ) ;
#2488 = CARTESIAN_POINT ( 'NONE',  ( 3.191455400233187412, 17.67480163422566619, -220.7055581859663107 ) ) ;
#2489 = CARTESIAN_POINT ( 'NONE',  ( -15.36327147092456791, 5.453733681707060299, -220.0043800961136355 ) ) ;
#2490 = CARTESIAN_POINT ( 'NONE',  ( -22.04004491965229207, 12.41871177236473578, -215.2165492276571115 ) ) ;
#2491 = CARTESIAN_POINT ( 'NONE',  ( -20.29356827505781879, -18.19569389227462253, -221.0297756488607490 ) ) ;
#2492 = CARTESIAN_POINT ( 'NONE',  ( 29.08100487150598212, 12.14819438347179670, -226.9621620069135020 ) ) ;
#2493 = CARTESIAN_POINT ( 'NONE',  ( -22.92944763917984830, 0.000000000000000000, -75.00000000000000000 ) ) ;
#2494 = CARTESIAN_POINT ( 'NONE',  ( -26.37829495954481374, -14.45191861565034053, -218.9345690753252711 ) ) ;
#2495 = CARTESIAN_POINT ( 'NONE',  ( -1.301562195391901877, 16.19210386685474390, -220.0867867038183192 ) ) ;
#2496 = CARTESIAN_POINT ( 'NONE',  ( 30.52813181070726856, 5.438803974502569361, -223.5441926215666513 ) ) ;
#2497 = CARTESIAN_POINT ( 'NONE',  ( -18.64931821476190876, 22.04453097546810270, -226.2485927806324923 ) ) ;
#2498 = CARTESIAN_POINT ( 'NONE',  ( 7.174260007897984792, 9.971262771497068300, -226.2872513832048469 ) ) ;
#2499 = ADVANCED_FACE ( 'NONE', ( #17315 ), #19432, .F. ) ;
#2500 = EDGE_LOOP ( 'NONE', ( #6718, #14451, #20486, #19386, #1651, #7087, #8905, #5065, #16599, #16028, #3097, #14085, #3262, #8443, #4239, #18996, #11919, #12097, #16271, #17566, #1885, #456, #13925, #4784, #8626, #14159 ) ) ;
#2501 = CARTESIAN_POINT ( 'NONE',  ( 5.786710755275625395, -21.74573425722988063, -218.5323380358915131 ) ) ;
#2502 = ORIENTED_EDGE ( 'NONE', *, *, #21773, .T. ) ;
#2503 = CARTESIAN_POINT ( 'NONE',  ( -0.1049609700611137120, -29.11428177772140558, -224.8408750893923411 ) ) ;
#2504 = CARTESIAN_POINT ( 'NONE',  ( 0.000000000000000000, 22.63401512838754570, -77.51594804401857175 ) ) ;
#2505 = CARTESIAN_POINT ( 'NONE',  ( 19.19288224840068935, 10.13059690604263174, -232.1906135022504998 ) ) ;
#2506 = CARTESIAN_POINT ( 'NONE',  ( 12.31511859722645852, -8.491226738247512174, -220.9006323875693738 ) ) ;
#2507 = CARTESIAN_POINT ( 'NONE',  ( -19.50907964299920039, -17.77536300509877876, -217.8007844881196320 ) ) ;
#2508 = CARTESIAN_POINT ( 'NONE',  ( -5.636842872076440081, -13.76003991320737541, -219.7405193562604495 ) ) ;
#2509 = CARTESIAN_POINT ( 'NONE',  ( 9.382249691333727881, 26.55946126407900820, -224.4468135941759215 ) ) ;
#2510 = DIRECTION ( 'NONE',  ( 0.000000000000000000, -1.000000000000000000, 0.000000000000000000 ) ) ;
#2511 = CARTESIAN_POINT ( 'NONE',  ( -12.79639481117843935, 1.974037863663017589, -229.6094308443170746 ) ) ;
#2512 = CARTESIAN_POINT ( 'NONE',  ( 3.449504654906655254, 27.59247159270940841, -231.3461799890608859 ) ) ;
#2513 = CARTESIAN_POINT ( 'NONE',  ( 3.174664235197445006, 17.30896320251298448, -221.0803896709622620 ) ) ;
#2514 = CARTESIAN_POINT ( 'NONE',  ( 13.34086609499694553, -4.728578536804411314, -230.1381470621469134 ) ) ;
#2515 = VERTEX_POINT ( 'NONE', #542 ) ;
#2516 = CARTESIAN_POINT ( 'NONE',  ( 12.74913679152205148, 9.185760885856177893, -218.6542381594888980 ) ) ;
#2517 = CARTESIAN_POINT ( 'NONE',  ( -14.67397018911906770, 9.031553917454052893, -228.4349422195089119 ) ) ;
#2518 = CARTESIAN_POINT ( 'NONE',  ( 29.00474534066713872, 11.29707752057770698, -221.8682176444242771 ) ) ;
#2519 = EDGE_CURVE ( 'NONE', #17072, #12912, #15637, .T. ) ;
#2520 = CARTESIAN_POINT ( 'NONE',  ( -7.182761810198031505, -27.78193072152378207, -222.3754761716870973 ) ) ;
#2521 = CARTESIAN_POINT ( 'NONE',  ( -17.50000000000000711, 0.000000000000000000, -30.00000000000000000 ) ) ;
#2522 = ORIENTED_EDGE ( 'NONE', *, *, #21445, .F. ) ;
#2523 = CARTESIAN_POINT ( 'NONE',  ( 17.60676319847677007, 21.31475060840986302, -219.8266339603936785 ) ) ;
#2524 = CARTESIAN_POINT ( 'NONE',  ( 14.80019294276752007, -6.608272808847591051, -224.1005182637183566 ) ) ;
#2525 = DIRECTION ( 'NONE',  ( 0.000000000000000000, 0.000000000000000000, 1.000000000000000000 ) ) ;
#2526 = CARTESIAN_POINT ( 'NONE',  ( -5.420780812268581883, -12.08122409751860360, -226.5143039284326392 ) ) ;
#2527 = APPLICATION_PROTOCOL_DEFINITION ( 'draft international standard', 'automotive_design', 1998, #15204 ) ;
#2528 = CARTESIAN_POINT ( 'NONE',  ( 1.217121169770782663, 15.31158828575123110, -230.6845728599757308 ) ) ;
#2529 = CARTESIAN_POINT ( 'NONE',  ( -1.302381543002304687, 18.65968181418110206, -215.1730913991678449 ) ) ;
#2530 = ORIENTED_EDGE ( 'NONE', *, *, #3918, .T. ) ;
#2531 = CARTESIAN_POINT ( 'NONE',  ( -6.101488798441174310, 11.33371047077072369, -225.3616985956418546 ) ) ;
#2532 = CARTESIAN_POINT ( 'NONE',  ( 23.56599333006272445, -4.960096179470117050, -217.5996013647105372 ) ) ;
#2533 = CARTESIAN_POINT ( 'NONE',  ( 0.000000000000000000, 0.000000000000000000, 69.99999999999998579 ) ) ;
#2534 = CARTESIAN_POINT ( 'NONE',  ( -20.99999999999999645, 0.000000000000000000, 60.00000000000001421 ) ) ;
#2535 = CARTESIAN_POINT ( 'NONE',  ( -6.282398543089500187, 12.01615879894893801, -228.5121145169883903 ) ) ;
#2536 = CARTESIAN_POINT ( 'NONE',  ( 4.470318609411144450, -14.75491745724135306, -219.7618428768379886 ) ) ;
#2537 = CARTESIAN_POINT ( 'NONE',  ( 25.69761320619099720, -8.403105518750903613, -219.2599777650661110 ) ) ;
#2538 = CARTESIAN_POINT ( 'NONE',  ( -9.151299407007059017, 9.196974979111923076, -223.9483834032048719 ) ) ;
#2539 = CARTESIAN_POINT ( 'NONE',  ( -31.12406087576577463, 7.316399946619934092, -225.0171288978685027 ) ) ;
#2540 = CARTESIAN_POINT ( 'NONE',  ( -2.129100187576105530, 26.11057959790866789, -231.5939360033278547 ) ) ;
#2541 = CARTESIAN_POINT ( 'NONE',  ( 0.000000000000000000, 0.000000000000000000, -70.00000000000000000 ) ) ;
#2542 = CARTESIAN_POINT ( 'NONE',  ( 27.94758519801750296, 7.894658480667867018, -227.3974864124137127 ) ) ;
#2543 = CARTESIAN_POINT ( 'NONE',  ( -18.43493186415240714, -20.29552032882516244, -227.2236339120829030 ) ) ;
#2544 = CARTESIAN_POINT ( 'NONE',  ( 12.08198696763335178, 15.54678077493410981, -216.6084679670902631 ) ) ;
#2545 = CARTESIAN_POINT ( 'NONE',  ( -21.01242583983345469, 16.60754347445175227, -220.8286358486543293 ) ) ;
#2546 = CARTESIAN_POINT ( 'NONE',  ( -15.33438615632468149, 23.56248205204123991, -229.2747191038674544 ) ) ;
#2547 = CARTESIAN_POINT ( 'NONE',  ( -26.22128172021140813, -2.843310382428120064, -218.3980250098940132 ) ) ;
#2548 = LINE ( 'NONE', #18093, #1397 ) ;
#2549 = ORIENTED_EDGE ( 'NONE', *, *, #7214, .F. ) ;
#2550 = CARTESIAN_POINT ( 'NONE',  ( -17.96792326766206926, -0.6237852504629022299, -217.9759415197746932 ) ) ;
#2551 = CARTESIAN_POINT ( 'NONE',  ( -3.607128793317693649, -14.45447024314366402, -228.6383918289709811 ) ) ;
#2552 = CARTESIAN_POINT ( 'NONE',  ( 13.96368202411823844, 1.657567506656081546, -227.5008844161029629 ) ) ;
#2553 = CARTESIAN_POINT ( 'NONE',  ( -4.104500432947460808, 15.73223271406093460, -218.0734292856946297 ) ) ;
#2554 = B_SPLINE_CURVE_WITH_KNOTS ( 'NONE', 3,
 ( #16647, #17902, #11364, #9458, #4366, #21473, #2465, #9348, #9676, #16208, #1007, #13049, #19897, #20008, #779, #21811, #16319, #4485, #11470, #895, #5957, #18233, #12834, #7771, #16535, #7989, #6289, #13163, #4594, #18677, #3131, #10122, #6511, #1341, #15418, #15085, #16763 ),
 .UNSPECIFIED., .F., .F.,
 ( 4, 1, 1, 1, 1, 2, 2, 1, 1, 1, 1, 1, 2, 2, 1, 1, 1, 1, 1, 2, 2, 1, 1, 1, 1, 1, 2, 4 ),
 ( 0.000000000000000000, 0.06249999999999955591, 0.09374999999999931999, 0.1093749999999992090, 0.1171874999999991673, 0.1210937499999991673, 0.1249999999999991673, 0.1874999999999990008, 0.2187499999999988898, 0.2343749999999988343, 0.2421874999999988065, 0.2460937499999987788, 0.2480468749999987510, 0.2499999999999987788, 0.3124999999999985012, 0.3437499999999983902, 0.3593749999999983347, 0.3671874999999983347, 0.3710937499999982792, 0.3730468749999982792, 0.3749999999999982792, 0.4374999999999991118, 0.4687499999999995559, 0.4843749999999997780, 0.4921874999999998890, 0.4960937499999998890, 0.4980468749999999445, 0.5000000000000000000 ),
 .UNSPECIFIED. ) ;
#2555 = FACE_OUTER_BOUND ( 'NONE', #14128, .T. ) ;
#2556 = CARTESIAN_POINT ( 'NONE',  ( -15.82952867276381603, 3.677461268355039170, -227.9997968350711801 ) ) ;
#2557 = CARTESIAN_POINT ( 'NONE',  ( 10.35958063030883025, 8.003303894222913328, -225.9303204057916048 ) ) ;
#2558 = CARTESIAN_POINT ( 'NONE',  ( 11.62313423782632782, 11.98467543564608029, -219.7293303032897995 ) ) ;
#2559 = DIRECTION ( 'NONE',  ( 0.000000000000000000, 0.000000000000000000, -1.000000000000000000 ) ) ;
#2560 = CARTESIAN_POINT ( 'NONE',  ( -30.36433721104044992, -10.30696067327809651, -227.5875578433412159 ) ) ;
#2561 = CARTESIAN_POINT ( 'NONE',  ( -20.83683780809167629, -19.66850649927503625, -219.7460615899071570 ) ) ;
#2562 = CARTESIAN_POINT ( 'NONE',  ( 8.709470447750865318, -17.43408031369701661, -216.5121658579468829 ) ) ;
#2563 = DIRECTION ( 'NONE',  ( -4.408728476930466911E-15, 1.000000000000000000, 0.000000000000000000 ) ) ;
#2564 = AXIS2_PLACEMENT_3D ( 'NONE', #463, #15664, #8383 ) ;
#2565 = DIRECTION ( 'NONE',  ( -1.000000000000000000, 0.000000000000000000, 0.000000000000000000 ) ) ;
#2566 = CARTESIAN_POINT ( 'NONE',  ( -12.19796877179171446, 17.24929682309303658, -234.5722138766719809 ) ) ;
#2567 = CARTESIAN_POINT ( 'NONE',  ( 11.82206472115893447, -5.594380913675770728, -219.9420363600394239 ) ) ;
#2568 = CARTESIAN_POINT ( 'NONE',  ( 14.34945462593695531, -6.128426910066905542, -229.1128190117150041 ) ) ;
#2569 = CARTESIAN_POINT ( 'NONE',  ( -12.06153928353927540, 8.661506524875534296, -226.8425068572842349 ) ) ;
#2570 = CARTESIAN_POINT ( 'NONE',  ( 8.821742718405863215, 10.82866050966069160, -221.4785132813277642 ) ) ;
#2571 = CARTESIAN_POINT ( 'NONE',  ( 11.21155440434494643, 24.57152134148167733, -221.7155903571010356 ) ) ;
#2572 = ADVANCED_FACE ( 'NONE', ( #16081 ), #7420, .F. ) ;
#2573 = ORIENTED_EDGE ( 'NONE', *, *, #12275, .T. ) ;
#2574 = CARTESIAN_POINT ( 'NONE',  ( 3.550474435626596037, -26.82390172985419952, -218.7255222707324549 ) ) ;
#2575 = DIRECTION ( 'NONE',  ( 0.000000000000000000, 0.000000000000000000, 1.000000000000000000 ) ) ;
#2576 = AXIS2_PLACEMENT_3D ( 'NONE', #12006, #18973, #14370 ) ;
#2577 = CARTESIAN_POINT ( 'NONE',  ( -3.309130212696198559, 28.80211350556483296, -217.4284252357080334 ) ) ;
#2578 = CARTESIAN_POINT ( 'NONE',  ( -4.531689447889125866, 14.11317536318881416, -231.6806015375303502 ) ) ;
#2579 = CARTESIAN_POINT ( 'NONE',  ( 14.29170853205465264, -5.149528714972483989, -227.7869631675187350 ) ) ;
#2580 = CARTESIAN_POINT ( 'NONE',  ( -3.326157069579807946, 13.92020081821418565, -220.5733722327383930 ) ) ;
#2581 = LINE ( 'NONE', #14647, #4356 ) ;
#2582 = AXIS2_PLACEMENT_3D ( 'NONE', #11523, #4313, #9844 ) ;
#2583 = CARTESIAN_POINT ( 'NONE',  ( -5.529079411693809121, 13.00503897727793401, -226.8014833675713646 ) ) ;
#2584 = CARTESIAN_POINT ( 'NONE',  ( 17.72360441613731652, -1.822637811265336749, -232.2813868768326984 ) ) ;
#2585 = CARTESIAN_POINT ( 'NONE',  ( -13.58874046263339608, 12.73011668665171392, -216.5659449791897941 ) ) ;
#2586 = CARTESIAN_POINT ( 'NONE',  ( 21.53262694368047647, 11.06794636811408594, -231.8394491640143826 ) ) ;
#2587 = DIRECTION ( 'NONE',  ( -1.000000000000000000, 0.000000000000000000, 0.000000000000000000 ) ) ;
#2588 = ORIENTED_EDGE ( 'NONE', *, *, #4728, .F. ) ;
#2589 = CARTESIAN_POINT ( 'NONE',  ( -1.565160934061885500, 18.19073094521525391, -232.0278805765578909 ) ) ;
#2590 = CARTESIAN_POINT ( 'NONE',  ( -16.76449091996730090, -6.021196472930381738, -231.5810252088758432 ) ) ;
#2591 = CARTESIAN_POINT ( 'NONE',  ( 12.71450444683213021, 7.595266944807587350, -224.4213778964231665 ) ) ;
#2592 = CARTESIAN_POINT ( 'NONE',  ( 1.444415905432371749, -18.02453083990606331, -216.1804672466811894 ) ) ;
#2593 = FACE_OUTER_BOUND ( 'NONE', #12316, .T. ) ;
#2594 = AXIS2_PLACEMENT_3D ( 'NONE', #7560, #14652, #13066 ) ;
#2595 = CARTESIAN_POINT ( 'NONE',  ( -13.88743542672353826, 10.36310385030668613, -230.6144170796622745 ) ) ;
#2596 = EDGE_CURVE ( 'NONE', #10013, #21551, #17214, .T. ) ;
#2597 =( NAMED_UNIT ( * ) SI_UNIT ( $, .STERADIAN. ) SOLID_ANGLE_UNIT ( ) );
#2598 = CARTESIAN_POINT ( 'NONE',  ( 11.29822263435752205, -11.23247557268489771, -230.2410575525588570 ) ) ;
#2599 = CARTESIAN_POINT ( 'NONE',  ( 9.094331215210646135, 23.85463374792894342, -219.7669638091879847 ) ) ;
#2600 = CARTESIAN_POINT ( 'NONE',  ( -15.30295614572244922, 9.661125001905515930, -218.8475896279880146 ) ) ;
#2601 = CARTESIAN_POINT ( 'NONE',  ( -9.722597143579921664, 7.159547510896417499, -227.5730737101346222 ) ) ;
#2602 = CARTESIAN_POINT ( 'NONE',  ( -14.57915343259292307, -9.548365625374035659, -229.2620333697842057 ) ) ;
#2603 = CARTESIAN_POINT ( 'NONE',  ( 10.02118533929671074, 10.65166262057242008, -217.7534731326719566 ) ) ;
#2604 = CARTESIAN_POINT ( 'NONE',  ( 1.322875655532295358, 1.500000000000000000, -105.0000000000000142 ) ) ;
#2605 = CARTESIAN_POINT ( 'NONE',  ( -26.65136949509196640, -16.37772123076025466, -229.1931346627563073 ) ) ;
#2606 = CARTESIAN_POINT ( 'NONE',  ( 7.163080459435270164, 24.05253566895842354, -232.4475987112033408 ) ) ;
#2607 = CIRCLE ( 'NONE', #5842, 2.999999999999999112 ) ;
#2608 = CARTESIAN_POINT ( 'NONE',  ( 14.50618777373884960, 4.375057440872940795, -230.8807389798650433 ) ) ;
#2609 = VECTOR ( 'NONE', #2075, 1000.000000000000000 ) ;
#2610 = CARTESIAN_POINT ( 'NONE',  ( -5.974114889119001681, 17.52937113675171332, -232.3862906442651592 ) ) ;
#2611 = CARTESIAN_POINT ( 'NONE',  ( 9.818699534354031755, 13.69084898312510390, -233.4870046949650089 ) ) ;
#2612 = CARTESIAN_POINT ( 'NONE',  ( 8.483411394722875087, -26.22410139474833457, -227.7697325675642617 ) ) ;
#2613 = ORIENTED_EDGE ( 'NONE', *, *, #4471, .T. ) ;
#2614 = CARTESIAN_POINT ( 'NONE',  ( -0.6703493356118243041, -28.01673786290986712, -221.2203946787553548 ) ) ;
#2615 = CARTESIAN_POINT ( 'NONE',  ( 18.60971343765040942, 2.368090295052050820, -218.6871071987073094 ) ) ;
#2616 = CARTESIAN_POINT ( 'NONE',  ( 11.90144651507291051, -8.898305237537579515, -228.5592478859710184 ) ) ;
#2617 = CARTESIAN_POINT ( 'NONE',  ( 13.49429091642815770, -0.3433647160923702368, -223.9641315955981895 ) ) ;
#2618 = CARTESIAN_POINT ( 'NONE',  ( -14.34280792637948743, -22.10828917559366147, -217.4172704053049756 ) ) ;
#2619 = CARTESIAN_POINT ( 'NONE',  ( 7.249842700832647147, 18.24319783868832801, -219.1110502051974720 ) ) ;
#2620 = CARTESIAN_POINT ( 'NONE',  ( 21.15841376125116824, 4.865517895153391947, -217.1795922978051578 ) ) ;
#2621 = CARTESIAN_POINT ( 'NONE',  ( 4.559463107227270662, 13.27337529356814017, -226.9596205199204633 ) ) ;
#2622 = CARTESIAN_POINT ( 'NONE',  ( 3.198229568054530070, 16.42319727383711481, -222.3960047798183552 ) ) ;
#2623 = CARTESIAN_POINT ( 'NONE',  ( 16.22685372911609036, -0.3790667790403521309, -218.4894315352551644 ) ) ;
#2624 = ORIENTED_EDGE ( 'NONE', *, *, #19790, .T. ) ;
#2625 = AXIS2_PLACEMENT_3D ( 'NONE', #18150, #9815, #11392 ) ;
#2626 = VECTOR ( 'NONE', #310, 1000.000000000000000 ) ;
#2627 = CARTESIAN_POINT ( 'NONE',  ( 17.24952650401854370, 25.19767938110938843, -224.5319471861414797 ) ) ;
#2628 = CARTESIAN_POINT ( 'NONE',  ( -13.41250421226414069, 17.27419134292087577, -217.6844171132545966 ) ) ;
#2629 = CARTESIAN_POINT ( 'NONE',  ( -27.56397725925346975, 4.259055856374357241, -222.4951663284069241 ) ) ;
#2630 = CARTESIAN_POINT ( 'NONE',  ( 4.788325992165110456, -24.70830725884669121, -218.5516572218182603 ) ) ;
#2631 = DIRECTION ( 'NONE',  ( -1.000000000000000000, 0.000000000000000000, 0.000000000000000000 ) ) ;
#2632 = CARTESIAN_POINT ( 'NONE',  ( 0.000000000000000000, 0.000000000000000000, -75.00000000000000000 ) ) ;
#2633 = EDGE_CURVE ( 'NONE', #15441, #11225, #10382, .T. ) ;
#2634 = CARTESIAN_POINT ( 'NONE',  ( 15.89706143421296147, 10.57416387607782227, -218.3862415393350318 ) ) ;
#2635 = CARTESIAN_POINT ( 'NONE',  ( 18.63320037895408277, -18.75851321891666146, -220.1409915463867151 ) ) ;
#2636 = CARTESIAN_POINT ( 'NONE',  ( -21.28183200535960040, 1.085030287403131233, -217.0000000015322712 ) ) ;
#2637 = CARTESIAN_POINT ( 'NONE',  ( -8.379125946468517938, -29.31735857037017468, -221.8060643354269814 ) ) ;
#2638 = PRODUCT_CONTEXT ( 'NONE', #9447, 'mechanical' ) ;
#2639 = CARTESIAN_POINT ( 'NONE',  ( 4.883314309504700468, 19.06839645569368358, -217.0171359871271193 ) ) ;
#2641 = CARTESIAN_POINT ( 'NONE',  ( -5.028549462823471039, 18.55099042571767143, -234.6264744246184648 ) ) ;
#2640 = AXIS2_PLACEMENT_3D ( 'NONE', #13593, #20431, #14833 ) ;
#2642 = ORIENTED_EDGE ( 'NONE', *, *, #14893, .T. ) ;
#2643 = CARTESIAN_POINT ( 'NONE',  ( -6.571166997218196748, 12.74865329367398736, -229.9840124400968762 ) ) ;
#2644 = CARTESIAN_POINT ( 'NONE',  ( 23.00003818093501806, -2.342406833639917085, -233.2756072794339843 ) ) ;
#2645 = CARTESIAN_POINT ( 'NONE',  ( 23.84888352507021736, -3.411310983279423947, -216.3556234003997645 ) ) ;
#2646 = CARTESIAN_POINT ( 'NONE',  ( -22.17655517979967783, 6.104744444143960891, -7.926958773079715748 ) ) ;
#2647 = CARTESIAN_POINT ( 'NONE',  ( -11.24282496690421596, 12.44430180464951086, -232.4405891940542404 ) ) ;
#2648 = CARTESIAN_POINT ( 'NONE',  ( -12.81114484120449504, -26.81657559919244349, -231.7433950434849805 ) ) ;
#2649 = CARTESIAN_POINT ( 'NONE',  ( 19.63495056682994289, -4.096126682090319271, -232.1271738766904207 ) ) ;
#2650 = CARTESIAN_POINT ( 'NONE',  ( -13.58874046263339608, 12.73011668665171392, -216.5659449791897941 ) ) ;
#2651 = CARTESIAN_POINT ( 'NONE',  ( 17.32394486779715592, 4.028159306070694612, -218.4253989884176690 ) ) ;
#2652 = CARTESIAN_POINT ( 'NONE',  ( 4.482815116226093188, 26.97722808566452812, -229.2080185206130238 ) ) ;
#2653 = DIRECTION ( 'NONE',  ( -1.000000000000000000, 0.000000000000000000, 0.000000000000000000 ) ) ;
#2654 = CARTESIAN_POINT ( 'NONE',  ( 21.91535456744164279, 7.573568724377624406, -232.0371228855588868 ) ) ;
#2655 = CARTESIAN_POINT ( 'NONE',  ( -8.785593564164850378, -26.69987990810942691, -222.9015467003982849 ) ) ;
#2656 = ORIENTED_EDGE ( 'NONE', *, *, #14942, .F. ) ;
#2657 = CARTESIAN_POINT ( 'NONE',  ( 9.798337081649805214, 12.27506320122302697, -218.9346733583377613 ) ) ;
#2658 = CARTESIAN_POINT ( 'NONE',  ( -6.260151855817680300, 29.88549235135308635, -226.8929519981915064 ) ) ;
#2659 = CARTESIAN_POINT ( 'NONE',  ( -14.78201816772319077, -5.155518158621814173, -222.1275223803717154 ) ) ;
#2660 = FACE_OUTER_BOUND ( 'NONE', #3609, .T. ) ;
#2661 = VERTEX_POINT ( 'NONE', #13953 ) ;
#2662 = CARTESIAN_POINT ( 'NONE',  ( 15.92396645628901020, -0.3225394686005420009, -223.0199929375764327 ) ) ;
#2663 = CARTESIAN_POINT ( 'NONE',  ( -5.077014288276974874, -29.41487918302398796, -226.0100937268998962 ) ) ;
#2664 = CARTESIAN_POINT ( 'NONE',  ( 14.19800769603076240, 4.587407146151301518, -224.2928935459285071 ) ) ;
#2665 = AXIS2_PLACEMENT_3D ( 'NONE', #9411, #17753, #7839 ) ;
#2666 = CARTESIAN_POINT ( 'NONE',  ( 5.248230734842167955, 23.54336384919183445, -216.8914391693808739 ) ) ;
#2667 = CARTESIAN_POINT ( 'NONE',  ( 14.85895087972432549, -2.358194654258901846, -226.8569002201626290 ) ) ;
#2668 = UNCERTAINTY_MEASURE_WITH_UNIT (LENGTH_MEASURE( 1.000000000000000082E-05 ), #5436, 'distance_accuracy_value', 'NONE');
#2669 = CARTESIAN_POINT ( 'NONE',  ( -24.19163806436329978, 8.131440952769249719, -230.9341214615949127 ) ) ;
#2670 = CARTESIAN_POINT ( 'NONE',  ( 22.90621760533471019, 17.25363305745006670, -230.8615280072714597 ) ) ;
#2671 = CARTESIAN_POINT ( 'NONE',  ( -17.50000000000000711, 0.000000000000000000, -24.99999999999999645 ) ) ;
#2672 = EDGE_CURVE ( 'NONE', #6212, #9522, #7164, .T. ) ;
#2673 = CARTESIAN_POINT ( 'NONE',  ( 20.41153371889344825, 17.18812948447019551, -230.7531656956970778 ) ) ;
#2674 = DIRECTION ( 'NONE',  ( -1.000000000000000000, 0.000000000000000000, 0.000000000000000000 ) ) ;
#2675 = CARTESIAN_POINT ( 'NONE',  ( 17.75464445068659458, -4.950329359371821170, -229.7529072665692240 ) ) ;
#2676 = CARTESIAN_POINT ( 'NONE',  ( -15.51091956967506391, -1.782849713491490018, -228.8089183834494520 ) ) ;
#2677 = CARTESIAN_POINT ( 'NONE',  ( -22.85322867788590528, -2.613756811604178942, -9.658044004399586768 ) ) ;
#2678 = CIRCLE ( 'NONE', #15285, 3.000000000000002665 ) ;
#2679 = DIRECTION ( 'NONE',  ( -1.000000000000000000, 0.000000000000000000, 0.000000000000000000 ) ) ;
#2680 = CARTESIAN_POINT ( 'NONE',  ( -9.290933312444883185, 29.15551353946876745, -225.8551562993724247 ) ) ;
#2681 = CARTESIAN_POINT ( 'NONE',  ( 23.82514222742702614, -14.35463969081363267, -233.5616060903067535 ) ) ;
#2682 = CARTESIAN_POINT ( 'NONE',  ( 20.25084204406298127, -10.11176871144018818, -232.7817218064674591 ) ) ;
#2683 = CARTESIAN_POINT ( 'NONE',  ( -19.74163224554151697, 8.726897413558679872, -232.6665747339030190 ) ) ;
#2684 = CARTESIAN_POINT ( 'NONE',  ( 22.73582563804385970, 20.20868311426415431, -227.8513184012435886 ) ) ;
#2685 = CARTESIAN_POINT ( 'NONE',  ( 20.92326490933994876, 18.00580109995737033, -222.6060933800056034 ) ) ;
#2686 = ORIENTED_EDGE ( 'NONE', *, *, #3303, .F. ) ;
#2687 = CARTESIAN_POINT ( 'NONE',  ( 3.098311947274309919, -13.44192016451707872, -223.0038505953381502 ) ) ;
#2688 = CARTESIAN_POINT ( 'NONE',  ( 19.20300624114736721, 0.6066039755357417462, -231.5046416827383950 ) ) ;
#2689 = CARTESIAN_POINT ( 'NONE',  ( -4.365576370787875859, 13.02741211227440665, -230.2897948137907917 ) ) ;
#2690 = CARTESIAN_POINT ( 'NONE',  ( -14.58084844870496966, 13.85720943031455832, -233.3219724312919254 ) ) ;
#2691 = CARTESIAN_POINT ( 'NONE',  ( 19.92157794555808437, -7.202678279460218214, -232.3584036642729416 ) ) ;
#2692 = CARTESIAN_POINT ( 'NONE',  ( -6.101488798441174310, 11.33371047077072369, -225.3616985956418546 ) ) ;
#2693 = CARTESIAN_POINT ( 'NONE',  ( -14.49031849020019003, -2.025093002184656488, 93.00000000000000000 ) ) ;
#2694 = VECTOR ( 'NONE', #13370, 1000.000000000000000 ) ;
#2695 = CARTESIAN_POINT ( 'NONE',  ( -5.786930954831501772, 15.78543306641166311, -231.0475152612371517 ) ) ;
#2696 = CARTESIAN_POINT ( 'NONE',  ( -16.66921372850992000, 0.4301828684420727078, -227.8397539831347842 ) ) ;
#2697 = CARTESIAN_POINT ( 'NONE',  ( -15.20262116893801974, 8.038155052917188570, -217.6767387945475036 ) ) ;
#2698 = CARTESIAN_POINT ( 'NONE',  ( 26.24002132888527328, 11.62331517472360964, -222.5300873157218859 ) ) ;
#2699 = CARTESIAN_POINT ( 'NONE',  ( 3.528957931946373971, 27.43889307663531696, -223.4805233499528185 ) ) ;
#2700 = CARTESIAN_POINT ( 'NONE',  ( 15.44208300017355739, 0.06603094323067049132, -228.0000000000006253 ) ) ;
#2701 = CARTESIAN_POINT ( 'NONE',  ( 7.951191770265756631, 20.55701948568933091, -231.2149185317973661 ) ) ;
#2702 = CARTESIAN_POINT ( 'NONE',  ( -15.74157322273402748, -13.22745315869835636, -216.7831660370879661 ) ) ;
#2703 = CARTESIAN_POINT ( 'NONE',  ( 14.98418162551161714, 4.450317369940187895, -227.9894155827521161 ) ) ;
#2704 = CARTESIAN_POINT ( 'NONE',  ( -3.535116539333309049, -19.81104435003528152, -216.2789031305144931 ) ) ;
#2705 = CARTESIAN_POINT ( 'NONE',  ( 0.000000000000000000, 0.000000000000000000, 93.00000000000000000 ) ) ;
#2706 = CARTESIAN_POINT ( 'NONE',  ( -12.05423124486310904, 12.38527783110887803, -219.7419643105747014 ) ) ;
#2707 = DIRECTION ( 'NONE',  ( 1.000000000000000000, 0.000000000000000000, 0.000000000000000000 ) ) ;
#2708 = CARTESIAN_POINT ( 'NONE',  ( 14.49023023880111083, -12.14520762395643061, -217.6171285705176501 ) ) ;
#2709 = CARTESIAN_POINT ( 'NONE',  ( 3.673290835002071653, 15.92545533070904895, -226.4848186297188022 ) ) ;
#2710 = CARTESIAN_POINT ( 'NONE',  ( -14.35594238341465889, 9.236863657925704629, -219.6542735655305307 ) ) ;
#2711 = CARTESIAN_POINT ( 'NONE',  ( -20.02994071726468661, 1.326980477106467271, -234.9527056834518532 ) ) ;
#2712 = CARTESIAN_POINT ( 'NONE',  ( -15.83567870103663466, -7.501751145129069265, -221.2716155488439824 ) ) ;
#2713 = COLOUR_RGB ( '', 0.66274510, 0.83137255, 0.94901961) ;
#2714 = CARTESIAN_POINT ( 'NONE',  ( 8.865150807857233417, 8.939496441981303221, -220.7647208555746090 ) ) ;
#2715 = CYLINDRICAL_SURFACE ( 'NONE', #487, 25.00000000000000000 ) ;
#2716 = CARTESIAN_POINT ( 'NONE',  ( -22.21568756412429835, -23.56320124644456016, -225.3776980696049463 ) ) ;
#2717 = CARTESIAN_POINT ( 'NONE',  ( 9.527502190795640757, 23.55559004943647139, -217.4101659741468211 ) ) ;
#2718 = CARTESIAN_POINT ( 'NONE',  ( 12.93042813863272755, 0.4488092930645843914, -225.5263188864764174 ) ) ;
#2719 = CARTESIAN_POINT ( 'NONE',  ( -13.23768812067001477, 12.78288831771969569, -230.4179793829127902 ) ) ;
#2720 = CARTESIAN_POINT ( 'NONE',  ( 7.116434306140963173, 9.967665124511082553, -224.4990387090310833 ) ) ;
#2721 = VECTOR ( 'NONE', #421, 1000.000000000000000 ) ;
#2722 = ORIENTED_EDGE ( 'NONE', *, *, #15991, .T. ) ;
#2723 = CARTESIAN_POINT ( 'NONE',  ( 0.005738405568439595983, -15.19016956849912070, -227.2100150994057230 ) ) ;
#2724 = CARTESIAN_POINT ( 'NONE',  ( -3.515149843921121509, -20.22121776728782550, -231.9652171757311123 ) ) ;
#2725 = CARTESIAN_POINT ( 'NONE',  ( 21.60524407607017849, 3.028118258437591415, -217.8361640396714449 ) ) ;
#2726 = CARTESIAN_POINT ( 'NONE',  ( 15.11994912051959972, -12.48385213956034079, -232.8079920308188377 ) ) ;
#2727 = CARTESIAN_POINT ( 'NONE',  ( -27.85133024402786006, -1.794102530182491773, -229.4204807338591081 ) ) ;
#2728 = CARTESIAN_POINT ( 'NONE',  ( -15.62091161899253855, -26.00636881980398840, -222.1463585103649905 ) ) ;
#2729 = CARTESIAN_POINT ( 'NONE',  ( 11.41090957555148222, 16.52772439454343711, -218.2458222691329013 ) ) ;
#2730 = CARTESIAN_POINT ( 'NONE',  ( 2.967317674205219191, -16.40215926535219282, -217.6245344443522924 ) ) ;
#2731 = CARTESIAN_POINT ( 'NONE',  ( 0.000000000000000000, 0.000000000000000000, -55.00000000000000000 ) ) ;
#2732 = CARTESIAN_POINT ( 'NONE',  ( -13.63442241228529994, 1.608023091903783008, -219.2326980015357094 ) ) ;
#2733 = CARTESIAN_POINT ( 'NONE',  ( 7.769483725421269860, 20.68783433326350263, -233.2348178266662728 ) ) ;
#2734 = CARTESIAN_POINT ( 'NONE',  ( 0.1979841192334154676, 16.22068729745496540, -223.9539336445596973 ) ) ;
#2735 = CARTESIAN_POINT ( 'NONE',  ( 8.798770371347417907, -12.71349942585338333, -232.9159113209695704 ) ) ;
#2736 = CARTESIAN_POINT ( 'NONE',  ( 11.63337745479824292, 8.229076005436313679, -220.5472098800687206 ) ) ;
#2737 = CARTESIAN_POINT ( 'NONE',  ( -18.64931821476190876, 22.04453097546810270, -226.2485927806324923 ) ) ;
#2738 = CARTESIAN_POINT ( 'NONE',  ( -27.01279207917464475, 4.316569700791554887, -221.4451031230926219 ) ) ;
#2739 = CARTESIAN_POINT ( 'NONE',  ( -0.6703493356118243041, -28.01673786290986712, -221.2203946787553548 ) ) ;
#2740 = CARTESIAN_POINT ( 'NONE',  ( 0.000000000000000000, 0.000000000000000000, -69.99999999999998579 ) ) ;
#2741 = CARTESIAN_POINT ( 'NONE',  ( 1.526556658859590243E-13, -22.63401512838748175, 77.51594804401857175 ) ) ;
#2742 = CARTESIAN_POINT ( 'NONE',  ( 22.84140515590350518, 18.29101041979067332, -226.2334522600520472 ) ) ;
#2743 = CARTESIAN_POINT ( 'NONE',  ( 13.30832375548903990, -9.333840824262514602, -222.9696809959601183 ) ) ;
#2744 = CARTESIAN_POINT ( 'NONE',  ( -18.88895772509644644, 1.306698388790553444, -217.6272550812279292 ) ) ;
#2745 = CARTESIAN_POINT ( 'NONE',  ( -5.279374154171231126, -12.28263746854076466, -222.5283095625445640 ) ) ;
#2746 = CARTESIAN_POINT ( 'NONE',  ( -2.934221234790329369, 15.07857928364152222, -230.9558365497803720 ) ) ;
#2747 = CARTESIAN_POINT ( 'NONE',  ( 4.065638640983322283, 32.08830473489500434, -226.0249194102539150 ) ) ;
#2748 = ORIENTED_EDGE ( 'NONE', *, *, #4317, .T. ) ;
#2749 = CARTESIAN_POINT ( 'NONE',  ( -12.78558550453068854, 7.693178343823584342, -230.0800953344970878 ) ) ;
#2750 = CARTESIAN_POINT ( 'NONE',  ( -13.68337831708448782, -3.656824064325736590, -221.3737413816871538 ) ) ;
#2751 = CARTESIAN_POINT ( 'NONE',  ( 30.39189047201120175, -1.943849802383817993, -228.0804048816970919 ) ) ;
#2752 = CARTESIAN_POINT ( 'NONE',  ( -22.85884317627467865, 2.625043582381284324, -9.671636207060540613 ) ) ;
#2753 = CARTESIAN_POINT ( 'NONE',  ( -9.250876228778270871, 9.538614635316015722, -227.1332118982684563 ) ) ;
#2754 = CARTESIAN_POINT ( 'NONE',  ( -22.21568756412429835, -23.56320124644456016, -225.3776980696049463 ) ) ;
#2755 = CARTESIAN_POINT ( 'NONE',  ( 22.44368505003003378, -11.72633196808685163, -232.1179326287041533 ) ) ;
#2756 = CARTESIAN_POINT ( 'NONE',  ( -12.31207293045244988, 6.732038552366256923, -221.0952066824360713 ) ) ;
#2757 = CARTESIAN_POINT ( 'NONE',  ( -11.84805200323110164, 5.835720598137266180, -228.2740675967047537 ) ) ;
#2758 = CARTESIAN_POINT ( 'NONE',  ( 2.482746429915354547, 16.41797261123590346, -229.5599230346982154 ) ) ;
#2759 = CARTESIAN_POINT ( 'NONE',  ( 0.000000000000000000, 0.000000000000000000, -30.00000000000000000 ) ) ;
#2760 = CARTESIAN_POINT ( 'NONE',  ( -19.59898341672158040, 3.279988180491820504, -234.9371679595475086 ) ) ;
#2761 = CARTESIAN_POINT ( 'NONE',  ( -13.20043892455957746, -23.63849784199488369, -228.2145582502841989 ) ) ;
#2762 = VERTEX_POINT ( 'NONE', #21336 ) ;
#2763 = CARTESIAN_POINT ( 'NONE',  ( -25.19248792833826300, 13.40115236862232528, -221.2817950683888455 ) ) ;
#2764 = CARTESIAN_POINT ( 'NONE',  ( 9.880827190695510964, 24.82036951119805579, -218.1633337467656020 ) ) ;
#2765 = CARTESIAN_POINT ( 'NONE',  ( -2.508488193221233953, 16.03207605874066033, -217.8880952293912969 ) ) ;
#2766 = ORIENTED_EDGE ( 'NONE', *, *, #18879, .F. ) ;
#2767 = CARTESIAN_POINT ( 'NONE',  ( 18.43413881788024611, -3.292634616013774274, -216.7808090690139409 ) ) ;
#2768 = CARTESIAN_POINT ( 'NONE',  ( 0.000000000000000000, 0.000000000000000000, -77.51594804401857175 ) ) ;
#2769 = EDGE_LOOP ( 'NONE', ( #21509, #11219, #17546, #11721 ) ) ;
#2770 = CARTESIAN_POINT ( 'NONE',  ( -24.02434186778878455, 18.57431834865475651, -228.2662945587547370 ) ) ;
#2771 = CARTESIAN_POINT ( 'NONE',  ( -4.832117640292445060, -22.41582585812286865, -216.8192401332019870 ) ) ;
#2772 = DIRECTION ( 'NONE',  ( 1.000000000000000000, 0.000000000000000000, 0.000000000000000000 ) ) ;
#2773 = CARTESIAN_POINT ( 'NONE',  ( 10.66614775643814994, 26.29080367171353672, -230.0818785118670178 ) ) ;
#2774 = DIRECTION ( 'NONE',  ( -0.000000000000000000, -0.000000000000000000, 1.000000000000000000 ) ) ;
#2775 = CARTESIAN_POINT ( 'NONE',  ( -12.30606003331388543, 10.59782772616791036, -231.0021630509705801 ) ) ;
#2776 = CARTESIAN_POINT ( 'NONE',  ( 17.88619020626327938, 19.43517936004721847, -216.7078103882350604 ) ) ;
#2777 = CARTESIAN_POINT ( 'NONE',  ( 15.48387324202036908, 0.7120489543666520538, -222.0826739725034997 ) ) ;
#2778 = CARTESIAN_POINT ( 'NONE',  ( 14.39473142419577023, 15.98257177912839389, -217.4557725731239373 ) ) ;
#2779 = CARTESIAN_POINT ( 'NONE',  ( 0.000000000000000000, 0.000000000000000000, 75.00000000000000000 ) ) ;
#2780 = CARTESIAN_POINT ( 'NONE',  ( 18.87161431088011199, -9.942086275362749248, -230.8324498438813350 ) ) ;
#2782 = ADVANCED_FACE ( 'NONE', ( #19982 ), #6262, .F. ) ;
#2781 = CARTESIAN_POINT ( 'NONE',  ( -16.64477864544768337, -2.947896226079009807, -219.6737919733007516 ) ) ;
#2783 = CARTESIAN_POINT ( 'NONE',  ( 0.000000000000000000, 19.80000000000006111, -78.50000000000000000 ) ) ;
#2784 = DIRECTION ( 'NONE',  ( -1.000000000000000000, 0.000000000000000000, 0.000000000000000000 ) ) ;
#2785 = CARTESIAN_POINT ( 'NONE',  ( -2.665457046508036942, 16.94988614842223029, -218.7621057649994896 ) ) ;
#2786 = CARTESIAN_POINT ( 'NONE',  ( 16.57791564354289093, -3.035441731457511949, -233.7002882787241163 ) ) ;
#2787 = CARTESIAN_POINT ( 'NONE',  ( 15.84759643368428428, -7.142586963752317608, -231.1761396821659673 ) ) ;
#2788 = CARTESIAN_POINT ( 'NONE',  ( -29.22672729369577738, 6.588740615114764054, -224.9915299386302934 ) ) ;
#2789 = CARTESIAN_POINT ( 'NONE',  ( 29.89309326230132058, 6.052383583152112223, -228.3539431708548477 ) ) ;
#2790 = CARTESIAN_POINT ( 'NONE',  ( 16.53859560591101641, 22.24348416270211359, -223.7250258089275974 ) ) ;
#2791 = VERTEX_POINT ( 'NONE', #12914 ) ;
#2792 = CARTESIAN_POINT ( 'NONE',  ( 13.17262855481386374, -26.22572064374609013, -230.8671443076513583 ) ) ;
#2793 = CARTESIAN_POINT ( 'NONE',  ( 14.80394259695730064, 1.224172658189580432, -225.4564070658925061 ) ) ;
#2794 = CARTESIAN_POINT ( 'NONE',  ( -20.73319232323294514, 5.144688277016327582, -214.6391322078443977 ) ) ;
#2795 = CARTESIAN_POINT ( 'NONE',  ( 7.116434306140963173, 9.967665124511082553, -224.4990387090310833 ) ) ;
#2796 = CARTESIAN_POINT ( 'NONE',  ( 4.952019330116582907, 28.88045068338265509, -217.6369327391592208 ) ) ;
#2797 = CARTESIAN_POINT ( 'NONE',  ( 13.38912848839664704, -8.011079660592983487, -223.8512906815321628 ) ) ;
#2798 = EDGE_CURVE ( 'NONE', #12893, #5175, #6147, .T. ) ;
#2799 = CARTESIAN_POINT ( 'NONE',  ( -2.817219543927646175, 14.13981714106644993, -229.6779615865167443 ) ) ;
#2800 = LINE ( 'NONE', #11256, #21622 ) ;
#2801 = CIRCLE ( 'NONE', #18270, 17.50000000000001066 ) ;
#2802 = ADVANCED_FACE ( 'NONE', ( #867 ), #4621, .T. ) ;
#2803 = CARTESIAN_POINT ( 'NONE',  ( -6.581016643627174645, 27.50493254600863935, -230.8763182197739070 ) ) ;
#2804 = CARTESIAN_POINT ( 'NONE',  ( -15.12838653695630420, 3.161599240781852949, -225.7834014684609656 ) ) ;
#2805 = CARTESIAN_POINT ( 'NONE',  ( -13.56774755469388616, 7.311522441667196226, -219.1912666243428021 ) ) ;
#2806 = CARTESIAN_POINT ( 'NONE',  ( 13.49011766416699842, 7.659170998773840111, -228.1905628957712793 ) ) ;
#2807 = CARTESIAN_POINT ( 'NONE',  ( 13.50603691942335693, 22.79443449215731832, -229.7689193854997995 ) ) ;
#2808 = CARTESIAN_POINT ( 'NONE',  ( 15.55281408287027922, 0.9489306161008197460, -227.8472323654694947 ) ) ;
#2809 = ORIENTED_EDGE ( 'NONE', *, *, #5897, .F. ) ;
#2810 = CARTESIAN_POINT ( 'NONE',  ( 11.27486163995310164, 25.12851252939060487, -222.6718455410222930 ) ) ;
#2811 = CARTESIAN_POINT ( 'NONE',  ( -17.58118739749173898, -8.238107657346720458, -217.5252134542318458 ) ) ;
#2812 = CARTESIAN_POINT ( 'NONE',  ( 20.23125423326388628, 7.836699765464857137, -217.8891354894872450 ) ) ;
#2813 = CARTESIAN_POINT ( 'NONE',  ( -0.4062606655315902371, -23.43967590431752512, -234.4451928229410100 ) ) ;
#2814 = DIRECTION ( 'NONE',  ( 0.000000000000000000, 0.000000000000000000, 1.000000000000000000 ) ) ;
#2815 = CARTESIAN_POINT ( 'NONE',  ( -7.873497077133136735, 15.44270125396616677, -230.2562282217168672 ) ) ;
#2816 = FILL_AREA_STYLE_COLOUR ( '', #2713 ) ;
#2817 = CARTESIAN_POINT ( 'NONE',  ( 11.72194121175188997, -15.95900783718691507, -217.6519982781775013 ) ) ;
#2818 = CARTESIAN_POINT ( 'NONE',  ( 8.645835506124264214, 12.38899589144949687, -223.4673650485651990 ) ) ;
#2819 = CARTESIAN_POINT ( 'NONE',  ( -7.965409144353247761, 13.56739834143082213, -221.6246244520798712 ) ) ;
#2821 = AXIS2_PLACEMENT_3D ( 'NONE', #21893, #4675, #16957 ) ;
#2820 = CARTESIAN_POINT ( 'NONE',  ( -14.08083899843152231, 10.81596681319144970, -234.3239311387574446 ) ) ;
#2822 = CARTESIAN_POINT ( 'NONE',  ( -19.42704602366333688, -5.151203963165301936, -219.4215732619585708 ) ) ;
#2823 = CARTESIAN_POINT ( 'NONE',  ( -16.23590288079963173, 0.2625226423351309513, -226.8300841971807813 ) ) ;
#2824 = PLANE ( 'NONE',  #5505 ) ;
#2825 = CARTESIAN_POINT ( 'NONE',  ( -10.70714119831929168, -8.316548062297686172, -219.3892619542279192 ) ) ;
#2826 = CARTESIAN_POINT ( 'NONE',  ( -2.692720963948733282, 24.67937284847025481, -218.0912907784291406 ) ) ;
#2827 = CARTESIAN_POINT ( 'NONE',  ( 21.52074627118099315, 8.791036694007010155, -215.9547738671300294 ) ) ;
#2828 = CARTESIAN_POINT ( 'NONE',  ( -17.65560862077320081, 21.92186454631220371, -221.3776075196718693 ) ) ;
#2829 = CARTESIAN_POINT ( 'NONE',  ( 11.78717493688862206, 28.63884142527983556, -229.7724827508652652 ) ) ;
#2830 = CARTESIAN_POINT ( 'NONE',  ( 3.112457940538468470, -21.91845672593830940, -231.6743386618371403 ) ) ;
#2831 = CARTESIAN_POINT ( 'NONE',  ( -2.389036117848273300, -16.12222041688038132, -229.2542492100865559 ) ) ;
#2832 = CARTESIAN_POINT ( 'NONE',  ( -18.67456582549428390, 11.07053394491094345, -214.7114755712704550 ) ) ;
#2833 = CARTESIAN_POINT ( 'NONE',  ( 21.39922646226391478, -21.53954253117021977, -224.1701659532164967 ) ) ;
#2834 = CARTESIAN_POINT ( 'NONE',  ( -14.48876282330270016, -2.056064607042531911, -223.6537127325441361 ) ) ;
#2835 = CARTESIAN_POINT ( 'NONE',  ( -5.519971913460887336, -12.21762732219001713, -227.2962593638428359 ) ) ;
#2836 = CARTESIAN_POINT ( 'NONE',  ( 26.51393280883522863, 15.12455065102723495, -226.1955201378414415 ) ) ;
#2837 = CARTESIAN_POINT ( 'NONE',  ( -16.23205080756887853, 1.987852906508643644E-15, 95.00000000000000000 ) ) ;
#2838 = CARTESIAN_POINT ( 'NONE',  ( -10.10782416658048710, 9.083762506436128703, -227.1045422723873344 ) ) ;
#2839 = CARTESIAN_POINT ( 'NONE',  ( -3.673551555920188783, 29.81207051619892923, -228.8770490300152005 ) ) ;
#2840 = CARTESIAN_POINT ( 'NONE',  ( 9.931717191100288389, 12.93133689537362940, -228.8926047089119038 ) ) ;
#2841 = CARTESIAN_POINT ( 'NONE',  ( 10.88145840916109819, -7.482884786208209960, -219.8679920012262414 ) ) ;
#2842 = CARTESIAN_POINT ( 'NONE',  ( 23.22505041959077232, 19.39625294115234055, -221.5972645870541555 ) ) ;
#2843 = CARTESIAN_POINT ( 'NONE',  ( -14.20363567091065349, 7.857660128015216294, -223.4151327167956822 ) ) ;
#2844 = CARTESIAN_POINT ( 'NONE',  ( -2.389036117848273300, -16.12222041688038132, -229.2542492100865559 ) ) ;
#2845 = DIRECTION ( 'NONE',  ( -0.000000000000000000, -0.000000000000000000, -1.000000000000000000 ) ) ;
#2846 = CARTESIAN_POINT ( 'NONE',  ( 25.50000000000000000, 0.5000000000000000000, -6.000000000000000000 ) ) ;
#2847 = CARTESIAN_POINT ( 'NONE',  ( 19.72515656911863147, 14.02277373989196541, -218.0718040828188009 ) ) ;
#2848 = CARTESIAN_POINT ( 'NONE',  ( 12.37559490515920579, -12.83230305503110991, -219.7713711637379106 ) ) ;
#2849 = CARTESIAN_POINT ( 'NONE',  ( -27.92885697401080591, 6.962042978589167319, -220.9552227796709190 ) ) ;
#2850 = CARTESIAN_POINT ( 'NONE',  ( -1.632242579688942596, -13.62074943359385415, -221.1585305289511041 ) ) ;
#2851 = CARTESIAN_POINT ( 'NONE',  ( -3.843007962268670585, 27.94983497691806917, -231.4302614368887703 ) ) ;
#2852 = CARTESIAN_POINT ( 'NONE',  ( 4.024086222410633518, 12.48004227094270746, -230.0177668608922374 ) ) ;
#2853 = VERTEX_POINT ( 'NONE', #17880 ) ;
#2854 = CARTESIAN_POINT ( 'NONE',  ( 0.6364901924797052857, 13.89978473517355617, -221.8840706290426397 ) ) ;
#2855 = CARTESIAN_POINT ( 'NONE',  ( -12.88620494227545343, -3.269292211592822461, -225.1464181993036391 ) ) ;
#2856 = CARTESIAN_POINT ( 'NONE',  ( -22.94181006055967131, -9.934448251827856069, -1.319932347539896966 ) ) ;
#2857 = CARTESIAN_POINT ( 'NONE',  ( 0.000000000000000000, 0.000000000000000000, 78.50000000000000000 ) ) ;
#2858 = CARTESIAN_POINT ( 'NONE',  ( 0.6364901924797052857, 13.89978473517355617, -221.8840706290426397 ) ) ;
#2859 = CARTESIAN_POINT ( 'NONE',  ( -6.776294192501696401, -30.39940938379458046, -221.2799938066956997 ) ) ;
#2860 = CARTESIAN_POINT ( 'NONE',  ( 22.14671607713456325, -14.13547298543019437, -218.1897693226341914 ) ) ;
#2861 = CARTESIAN_POINT ( 'NONE',  ( -3.514547081416551588, 30.38636916157537016, -227.3529586180979436 ) ) ;
#2862 = CARTESIAN_POINT ( 'NONE',  ( -14.99655511003079233, 2.316638599135941945, -232.4215266639120046 ) ) ;
#2863 = CARTESIAN_POINT ( 'NONE',  ( 5.142103055192286831, 28.18228231877369439, -225.8998064704803994 ) ) ;
#2864 = CARTESIAN_POINT ( 'NONE',  ( -20.26851768784797869, -0.8260594303982465858, -217.1279713726092098 ) ) ;
#2865 = CARTESIAN_POINT ( 'NONE',  ( -14.01966324001334385, 10.60695606488527964, -217.6333332521996340 ) ) ;
#2866 = CARTESIAN_POINT ( 'NONE',  ( -12.19937816677273013, -10.70901586236097636, -226.3808855409166370 ) ) ;
#2867 = VERTEX_POINT ( 'NONE', #14502 ) ;
#2868 = EDGE_CURVE ( 'NONE', #6745, #4083, #2548, .T. ) ;
#2869 = CARTESIAN_POINT ( 'NONE',  ( -13.75208518020500748, 5.661250135068270239, -227.6647651141479685 ) ) ;
#2870 = CARTESIAN_POINT ( 'NONE',  ( 6.040050017043670394, 13.67534390435379699, -220.4759402345340504 ) ) ;
#2871 = CARTESIAN_POINT ( 'NONE',  ( -1.884624261322229266, 13.00421381464247084, -226.7648460381863345 ) ) ;
#2872 = CARTESIAN_POINT ( 'NONE',  ( -18.30524310960561252, -4.731645231655051909, -231.4308113063693781 ) ) ;
#2873 = CARTESIAN_POINT ( 'NONE',  ( 0.000000000000000000, 0.000000000000000000, -77.51594804401857175 ) ) ;
#2874 = ORIENTED_EDGE ( 'NONE', *, *, #19438, .T. ) ;
#2875 = CARTESIAN_POINT ( 'NONE',  ( -10.51143808951550085, 11.41308718311005066, -231.3573069600382439 ) ) ;
#2876 = CARTESIAN_POINT ( 'NONE',  ( -20.07469464351956390, -22.83895492621963896, -220.1373730632280967 ) ) ;
#2877 = CARTESIAN_POINT ( 'NONE',  ( 13.64549276890110008, 1.404530603506124020, -227.6530344292614245 ) ) ;
#2878 = CARTESIAN_POINT ( 'NONE',  ( 15.12287735332712835, 21.03907941686458116, -231.7894952627153202 ) ) ;
#2879 = DIRECTION ( 'NONE',  ( 0.000000000000000000, 0.000000000000000000, 1.000000000000000000 ) ) ;
#2880 = PRODUCT_DEFINITION_CONTEXT ( 'detailed design', #5984, 'design' ) ;
#2881 = CARTESIAN_POINT ( 'NONE',  ( 28.33476664927451338, -0.7768526459456059907, -228.3750448408243869 ) ) ;
#2882 = CARTESIAN_POINT ( 'NONE',  ( -13.66744685701839046, 5.938820276054873837, -223.0954633396572149 ) ) ;
#2883 = CARTESIAN_POINT ( 'NONE',  ( 15.46952826979347151, 3.173892190046953665, -221.7237849701489552 ) ) ;
#2884 = CARTESIAN_POINT ( 'NONE',  ( 13.92641534307036189, 0.2825193253608765387, -222.0121013341077969 ) ) ;
#2885 = CARTESIAN_POINT ( 'NONE',  ( 19.08116649778970952, -2.725278401796281447, -223.7411956188273621 ) ) ;
#2886 = DIRECTION ( 'NONE',  ( -1.000000000000000000, -0.000000000000000000, -0.000000000000000000 ) ) ;
#2887 = CARTESIAN_POINT ( 'NONE',  ( 20.53331905177824979, -5.913034700419025569, -230.9395893631423462 ) ) ;
#2888 = AXIS2_PLACEMENT_3D ( 'NONE', #4214, #14918, #840 ) ;
#2889 = CARTESIAN_POINT ( 'NONE',  ( -26.07210576407111446, -8.413030596423759278, -230.6002792590230115 ) ) ;
#2890 = CARTESIAN_POINT ( 'NONE',  ( 2.465190328815661892E-29, 25.00000000000012790, 75.00000000000000000 ) ) ;
#2891 = DIRECTION ( 'NONE',  ( -0.000000000000000000, -0.000000000000000000, -1.000000000000000000 ) ) ;
#2892 = CARTESIAN_POINT ( 'NONE',  ( -11.23881320317003407, 15.84151802331611236, -234.2799649731619809 ) ) ;
#2893 = CARTESIAN_POINT ( 'NONE',  ( 30.30402220111207612, -9.997565949388443229, -221.8870099070453250 ) ) ;
#2894 = CARTESIAN_POINT ( 'NONE',  ( 28.78651053433536333, -0.9604905981993369091, -227.3547688931310233 ) ) ;
#2895 = CARTESIAN_POINT ( 'NONE',  ( -14.35594238341465889, 9.236863657925704629, -219.6542735655305307 ) ) ;
#2896 = CARTESIAN_POINT ( 'NONE',  ( 15.39025625686376841, 1.044190007782545226, -218.9203249718910911 ) ) ;
#2897 = CARTESIAN_POINT ( 'NONE',  ( 12.91676121433235913, 9.519065828383201477, -226.8102878246443765 ) ) ;
#2898 = CARTESIAN_POINT ( 'NONE',  ( -0.7782973328492528431, -21.73504563028646075, -232.5926793935175283 ) ) ;
#2899 = DIRECTION ( 'NONE',  ( 0.000000000000000000, 0.000000000000000000, -1.000000000000000000 ) ) ;
#2900 = CARTESIAN_POINT ( 'NONE',  ( -20.06846544527470400, 7.877362284741439069, -235.3910773253824402 ) ) ;
#2901 = CARTESIAN_POINT ( 'NONE',  ( 19.66122710937851537, 22.83208755991274330, -220.0578523118790883 ) ) ;
#2902 = CARTESIAN_POINT ( 'NONE',  ( 3.982203626615636427, 14.63895582687697150, -217.4952312584269123 ) ) ;
#2903 = CARTESIAN_POINT ( 'NONE',  ( 24.22993967103762714, -2.502297861120115208, -232.9814837474525007 ) ) ;
#2904 = CARTESIAN_POINT ( 'NONE',  ( -7.913358619554302642, 16.16796202616373890, -233.0981776325470491 ) ) ;
#2905 = CARTESIAN_POINT ( 'NONE',  ( -24.48580119005125866, 9.312492396273500006, -232.5498413856076070 ) ) ;
#2906 = EDGE_CURVE ( 'NONE', #1838, #4211, #5700, .T. ) ;
#2907 = CARTESIAN_POINT ( 'NONE',  ( 16.71363093372661979, 20.70203100498337179, -215.6856694095356488 ) ) ;
#2908 = CARTESIAN_POINT ( 'NONE',  ( -15.60078324628501356, 3.527872497691606934, -227.4630248446626695 ) ) ;
#2909 = CARTESIAN_POINT ( 'NONE',  ( -24.48580119005125866, 9.312492396273500006, -232.5498413856076070 ) ) ;
#2910 = CARTESIAN_POINT ( 'NONE',  ( 14.54149994592679107, 8.070685273005897997, -229.7292930672863349 ) ) ;
#2911 = CARTESIAN_POINT ( 'NONE',  ( 8.632180352507942800, 16.83956698119041917, -230.4752415867875186 ) ) ;
#2912 = DIRECTION ( 'NONE',  ( 0.000000000000000000, 0.000000000000000000, 1.000000000000000000 ) ) ;
#2913 = FACE_OUTER_BOUND ( 'NONE', #3821, .T. ) ;
#2914 = EDGE_CURVE ( 'NONE', #18650, #10973, #5339, .T. ) ;
#2915 = CARTESIAN_POINT ( 'NONE',  ( -10.42804209284631156, -14.08702332024887305, -217.7386024361820489 ) ) ;
#2916 = CARTESIAN_POINT ( 'NONE',  ( 18.76922974182421555, 13.12635134380198210, -217.8010375391909008 ) ) ;
#2917 = CARTESIAN_POINT ( 'NONE',  ( -1.925327751674894339, -31.30071588347811584, -225.0681195224254623 ) ) ;
#2918 = DIRECTION ( 'NONE',  ( -1.000000000000000000, 0.000000000000000000, 0.000000000000000000 ) ) ;
#2919 = AXIS2_PLACEMENT_3D ( 'NONE', #18211, #7637, #2772 ) ;
#2920 = CARTESIAN_POINT ( 'NONE',  ( -6.720912670637915198, 19.69156892798266512, -217.8848069150180891 ) ) ;
#2921 = CARTESIAN_POINT ( 'NONE',  ( 12.70013114424463296, -16.94540864491495924, -217.3462533088837745 ) ) ;
#2922 = CARTESIAN_POINT ( 'NONE',  ( 8.812670488384366507, 12.21486833790445914, -225.9961634525829197 ) ) ;
#2923 = CARTESIAN_POINT ( 'NONE',  ( -4.742143146070755932, 15.01230778631049567, -221.4832709320255049 ) ) ;
#2924 = CARTESIAN_POINT ( 'NONE',  ( -28.12586305337175219, 12.75764838638491305, -230.3810511299127768 ) ) ;
#2925 = CARTESIAN_POINT ( 'NONE',  ( -14.94274040728286046, -6.247332224397157852, -226.1562440284360491 ) ) ;
#2926 = CARTESIAN_POINT ( 'NONE',  ( 17.72360441613731652, -1.822637811265336749, -232.2813868768326984 ) ) ;
#2927 = TOROIDAL_SURFACE ( 'NONE', #15887, 24.63401512838747820, 3.000000000000000888 ) ;
#2928 = CARTESIAN_POINT ( 'NONE',  ( -23.00000000000000355, 0.000000000000000000, 75.00000000000000000 ) ) ;
#2929 = CARTESIAN_POINT ( 'NONE',  ( 22.03647168421188240, 0.3315607655626218175, -232.0572713672587213 ) ) ;
#2930 = CARTESIAN_POINT ( 'NONE',  ( 11.09231067055629616, 7.417581979752235100, -227.5152062457793534 ) ) ;
#2931 = CARTESIAN_POINT ( 'NONE',  ( -16.27736488614644372, 5.941157768540612949, -228.4237983497913547 ) ) ;
#2932 = VECTOR ( 'NONE', #16594, 1000.000000000000000 ) ;
#2933 = CARTESIAN_POINT ( 'NONE',  ( 5.030854775705693172, 19.94152319263364603, -234.9034581965229336 ) ) ;
#2934 = CARTESIAN_POINT ( 'NONE',  ( 3.641537757978871248, 12.43698445400491437, -220.3805014257186485 ) ) ;
#2935 = CARTESIAN_POINT ( 'NONE',  ( -7.509561119170069077, -14.53281319394193538, -217.7574163112487042 ) ) ;
#2936 = TOROIDAL_SURFACE ( 'NONE', #20926, 24.63401512838747820, 3.000000000000000888 ) ;
#2937 = VERTEX_POINT ( 'NONE', #2442 ) ;
#2938 = CARTESIAN_POINT ( 'NONE',  ( 2.641673488600395636, -17.65289918763021149, -219.1873688300129288 ) ) ;
#2939 = EDGE_CURVE ( 'NONE', #2334, #20174, #21148, .T. ) ;
#2940 = CARTESIAN_POINT ( 'NONE',  ( -26.09112266552012471, 5.807188091516064077, -215.7774933166620883 ) ) ;
#2941 = CARTESIAN_POINT ( 'NONE',  ( 25.69672030403964769, -15.30292110028031338, -224.0206579222720791 ) ) ;
#2942 = CARTESIAN_POINT ( 'NONE',  ( 28.89510310306777541, -0.2847990887752292477, -220.1812426115722303 ) ) ;
#2943 = CARTESIAN_POINT ( 'NONE',  ( -11.07688804854283049, -12.81333559660784971, -232.1241261852632363 ) ) ;
#2944 = CARTESIAN_POINT ( 'NONE',  ( 20.88350594575732799, 13.65521425050155813, -232.8060468608549911 ) ) ;
#2945 = CARTESIAN_POINT ( 'NONE',  ( -22.00000000000137490, -2.602085213965210642E-15, -216.9999999999999716 ) ) ;
#2946 = CARTESIAN_POINT ( 'NONE',  ( -11.88513743913613752, 17.65694776598872195, -232.6054623148957035 ) ) ;
#2947 = CARTESIAN_POINT ( 'NONE',  ( 15.15306935214909778, 7.771180183537883757, -217.5526096523957165 ) ) ;
#2948 = CARTESIAN_POINT ( 'NONE',  ( 12.18657022793382794, 26.76558097653315471, -221.8882195427397335 ) ) ;
#2949 = CARTESIAN_POINT ( 'NONE',  ( 20.40268796714816801, 18.65534563792085621, -219.5587498978784993 ) ) ;
#2950 = CARTESIAN_POINT ( 'NONE',  ( 27.71804559688024128, -15.88771542466010978, -225.5747850090131692 ) ) ;
#2951 = CARTESIAN_POINT ( 'NONE',  ( 27.69955354773053458, 12.81264626165819287, -221.7750850138309602 ) ) ;
#2952 = CARTESIAN_POINT ( 'NONE',  ( -14.60180519431160917, 24.46340507526420893, -221.8423643191928534 ) ) ;
#2953 = CARTESIAN_POINT ( 'NONE',  ( -6.593106361191484410, 26.27107262772703322, -231.8730401762632596 ) ) ;
#2954 = CARTESIAN_POINT ( 'NONE',  ( -7.786003226018990198, -12.23758553950863082, -224.1954257758910671 ) ) ;
#2955 = CARTESIAN_POINT ( 'NONE',  ( -18.46722752239034193, 0.9784074152395518809, -232.1633353206286188 ) ) ;
#2956 = CIRCLE ( 'NONE', #14142, 23.00000000000008882 ) ;
#2957 = PLANE ( 'NONE',  #2582 ) ;
#2958 = AXIS2_PLACEMENT_3D ( 'NONE', #14735, #19446, #4033 ) ;
#2959 = CARTESIAN_POINT ( 'NONE',  ( 22.02796522526679723, 16.41909032291435366, -220.1590600991317217 ) ) ;
#2960 = CARTESIAN_POINT ( 'NONE',  ( 11.44298997664856721, -19.26084286805135193, -217.6324489131326914 ) ) ;
#2961 = CARTESIAN_POINT ( 'NONE',  ( -17.99720854823001659, 13.97888873227035056, -232.2992184661552244 ) ) ;
#2962 = CARTESIAN_POINT ( 'NONE',  ( -9.625604265899946554, -19.21123364792547505, -233.9327940972253259 ) ) ;
#2963 = CARTESIAN_POINT ( 'NONE',  ( -16.04492519386327487, 1.819644280589142626, -223.4665098021627614 ) ) ;
#2964 = CARTESIAN_POINT ( 'NONE',  ( 3.490345297502855715, 11.17751288514984331, -224.7799703251421022 ) ) ;
#2965 = VERTEX_POINT ( 'NONE', #19869 ) ;
#2966 = CARTESIAN_POINT ( 'NONE',  ( 0.4042326456706432647, 15.50845657815858303, -219.2680337625893401 ) ) ;
#2967 = CARTESIAN_POINT ( 'NONE',  ( -28.43596199216294806, -10.51226423640377838, -227.0041752157952430 ) ) ;
#2968 = CARTESIAN_POINT ( 'NONE',  ( -22.91279148301329016, -10.00019932322032723, 0.3240289003878054630 ) ) ;
#2969 = CARTESIAN_POINT ( 'NONE',  ( 0.000000000000000000, 17.50000000000000711, -55.00000000000000000 ) ) ;
#2970 = CARTESIAN_POINT ( 'NONE',  ( 0.9046320824004248085, 13.39785254849979701, -226.4815711199935890 ) ) ;
#2971 = CARTESIAN_POINT ( 'NONE',  ( -4.907461209876205821, -14.28794023480369368, -232.2749568027591636 ) ) ;
#2972 = CARTESIAN_POINT ( 'NONE',  ( 7.080148886126969465, -28.65852557119563926, -219.9679292432588227 ) ) ;
#2973 = AXIS2_PLACEMENT_3D ( 'NONE', #4346, #8804, #6153 ) ;
#2974 = DIRECTION ( 'NONE',  ( 0.000000000000000000, 0.000000000000000000, 1.000000000000000000 ) ) ;
#2975 = AXIS2_PLACEMENT_3D ( 'NONE', #19668, #5948, #6056 ) ;
#2976 = CARTESIAN_POINT ( 'NONE',  ( -13.96653539523557619, 20.94398119165846239, -231.8597527081015528 ) ) ;
#2977 = CARTESIAN_POINT ( 'NONE',  ( 13.55451907249704213, 16.71566520821242818, -219.1474322952048226 ) ) ;
#2978 = CARTESIAN_POINT ( 'NONE',  ( 22.00000000000000000, 6.162975822039154730E-30, -228.0000000000000000 ) ) ;
#2979 = CARTESIAN_POINT ( 'NONE',  ( -29.50764134580612463, 7.783340782857166573, -219.9768238800827191 ) ) ;
#2980 = CARTESIAN_POINT ( 'NONE',  ( -21.98560163549725033, -7.841739570055646702, -218.0982455035688474 ) ) ;
#2981 = ORIENTED_EDGE ( 'NONE', *, *, #8744, .T. ) ;
#2982 = CARTESIAN_POINT ( 'NONE',  ( -4.466732464217805898, 19.42663028452474450, -231.9485309169485561 ) ) ;
#2983 = CARTESIAN_POINT ( 'NONE',  ( 13.19406830060760605, 4.163358546877222288, -228.8532745215267425 ) ) ;
#2984 = CARTESIAN_POINT ( 'NONE',  ( 3.137667653003819446, 15.44806861187908176, -232.6841782316817842 ) ) ;
#2985 = CARTESIAN_POINT ( 'NONE',  ( 19.19076252585518105, -11.68002947460017715, -233.4322573972352188 ) ) ;
#2986 = CARTESIAN_POINT ( 'NONE',  ( 26.00000000000000000, 1.360023205165816762E-13, 0.000000000000000000 ) ) ;
#2987 = ORIENTED_EDGE ( 'NONE', *, *, #8940, .T. ) ;
#2988 = CARTESIAN_POINT ( 'NONE',  ( -24.24202834850560606, 19.05981756344202438, -226.6980666352953335 ) ) ;
#2989 = CARTESIAN_POINT ( 'NONE',  ( -10.66474234094022755, -20.68992156881482813, -215.8674331684499634 ) ) ;
#2990 = CYLINDRICAL_SURFACE ( 'NONE', #10486, 2.100000000000000089 ) ;
#2991 = CARTESIAN_POINT ( 'NONE',  ( 14.39473142419577023, 15.98257177912839389, -217.4557725731239373 ) ) ;
#2992 = LINE ( 'NONE', #4575, #19523 ) ;
#2993 = AXIS2_PLACEMENT_3D ( 'NONE', #7756, #767, #11236 ) ;
#2994 = CIRCLE ( 'NONE', #17751, 21.80000000000008598 ) ;
#2995 = FACE_OUTER_BOUND ( 'NONE', #18266, .T. ) ;
#2996 = CARTESIAN_POINT ( 'NONE',  ( -14.95675039876920032, 11.42095949000369259, -217.2220932760075129 ) ) ;
#2997 = CARTESIAN_POINT ( 'NONE',  ( 25.85597688020959239, 3.954559836939000039, -230.6766427064781624 ) ) ;
#2998 =( LENGTH_UNIT ( ) NAMED_UNIT ( * ) SI_UNIT ( .MILLI., .METRE. ) );
#2999 = CARTESIAN_POINT ( 'NONE',  ( 14.72991611006397861, 0.1487069797637389501, -222.0036671020463359 ) ) ;
#3000 = CARTESIAN_POINT ( 'NONE',  ( 19.24993070808567097, -2.578473320807608715, -223.4513235704932299 ) ) ;
#3001 = CARTESIAN_POINT ( 'NONE',  ( 1.526556658859591000E-13, -22.63401512838754570, -77.51594804401857175 ) ) ;
#3002 = CARTESIAN_POINT ( 'NONE',  ( 15.95205345792057550, -4.116367354408478896, -227.2937718740910498 ) ) ;
#3003 = CARTESIAN_POINT ( 'NONE',  ( -15.89118508636071958, -1.798691612803976492, -229.3605869667087234 ) ) ;
#3004 = CARTESIAN_POINT ( 'NONE',  ( 21.82657638218437057, -0.1729100361068852398, -227.9962408443968798 ) ) ;
#3005 = FACE_OUTER_BOUND ( 'NONE', #8881, .T. ) ;
#3006 = CARTESIAN_POINT ( 'NONE',  ( 10.48640380280471618, 25.27581435651469022, -227.8976696013017715 ) ) ;
#3007 = CARTESIAN_POINT ( 'NONE',  ( 4.565444334214069144, -15.90021673156186388, -218.4840512714275462 ) ) ;
#3008 = CARTESIAN_POINT ( 'NONE',  ( 9.358654279681809740, -11.94480763145079472, -229.8864256833185777 ) ) ;
#3009 = CARTESIAN_POINT ( 'NONE',  ( -20.71192633727912380, 6.339941255257877550, -217.2401662359725094 ) ) ;
#3010 = CARTESIAN_POINT ( 'NONE',  ( -16.98287383830707142, 1.584866439881522648, -221.5391863673846444 ) ) ;
#3011 = CARTESIAN_POINT ( 'NONE',  ( 13.80707869872719762, 6.429545566348308760, -225.7152177910682553 ) ) ;
#3012 = ORIENTED_EDGE ( 'NONE', *, *, #250, .T. ) ;
#3013 = AXIS2_PLACEMENT_3D ( 'NONE', #3894, #14047, #13709 ) ;
#3014 = CARTESIAN_POINT ( 'NONE',  ( 4.683166109028750412, -21.42534054955530110, -233.6038185840237986 ) ) ;
#3015 = CARTESIAN_POINT ( 'NONE',  ( 7.354678144329572120, -7.869443266638024070, 92.00000000000000000 ) ) ;
#3016 = CARTESIAN_POINT ( 'NONE',  ( -26.09112266552012471, 5.807188091516064077, -215.7774933166620883 ) ) ;
#3017 = CARTESIAN_POINT ( 'NONE',  ( 19.20222574149634909, 21.83532798770326266, -218.6913543321078919 ) ) ;
#3018 = CARTESIAN_POINT ( 'NONE',  ( -0.2758005215353623862, 11.79991891162212525, -226.8645588387054488 ) ) ;
#3019 = CARTESIAN_POINT ( 'NONE',  ( 15.93530172229541364, -10.24337635388110890, -230.8272463582829630 ) ) ;
#3020 = CARTESIAN_POINT ( 'NONE',  ( -6.201839134465864767, 11.37481922992157379, -223.7040893475979146 ) ) ;
#3021 = CARTESIAN_POINT ( 'NONE',  ( -15.82069055112642353, 8.315535108674763976, -217.2800172218543935 ) ) ;
#3022 = CARTESIAN_POINT ( 'NONE',  ( 7.283976506941576723, 24.82246917020504284, -234.3244871078919402 ) ) ;
#3023 = CARTESIAN_POINT ( 'NONE',  ( -22.70558257617108922, 14.65737936663030538, -230.9775454010380997 ) ) ;
#3024 = CARTESIAN_POINT ( 'NONE',  ( -8.501641725227710111, 25.47064987787527102, -217.3358698761548737 ) ) ;
#3025 = AXIS2_PLACEMENT_3D ( 'NONE', #12759, #20022, #17720 ) ;
#3026 = CARTESIAN_POINT ( 'NONE',  ( 8.476473295508071715, 6.680697330908218490, 92.00000000000002842 ) ) ;
#3027 = CARTESIAN_POINT ( 'NONE',  ( 7.249842700832647147, 18.24319783868832801, -219.1110502051974720 ) ) ;
#3028 = CARTESIAN_POINT ( 'NONE',  ( 25.69761320619099720, -8.403105518750903613, -219.2599777650661110 ) ) ;
#3029 = CARTESIAN_POINT ( 'NONE',  ( 0.000000000000000000, 24.63401512838747820, -77.51594804401857175 ) ) ;
#3030 = CARTESIAN_POINT ( 'NONE',  ( 1.665334536937734811E-13, -23.00000000000000000, 69.99999999999998579 ) ) ;
#3031 = CARTESIAN_POINT ( 'NONE',  ( 21.60524407607017849, 3.028118258437591415, -217.8361640396714449 ) ) ;
#3032 = CARTESIAN_POINT ( 'NONE',  ( -15.97267037792306255, -23.58045393237649279, -221.6247985403941527 ) ) ;
#3033 = CARTESIAN_POINT ( 'NONE',  ( 19.66230024959844513, 2.213945732971074332, -227.0341823791074773 ) ) ;
#3034 = ADVANCED_FACE ( 'NONE', ( #2660 ), #12697, .F. ) ;
#3035 = CARTESIAN_POINT ( 'NONE',  ( -16.84845737324940984, 22.31296517946017488, -228.8910390263689010 ) ) ;
#3036 = CARTESIAN_POINT ( 'NONE',  ( 18.70674991763376482, -20.04093309878971496, -230.8534322170362714 ) ) ;
#3037 = CARTESIAN_POINT ( 'NONE',  ( 11.54460987479198053, 9.649171130674412566, -228.7280371210653698 ) ) ;
#3038 = CARTESIAN_POINT ( 'NONE',  ( -7.464187997994982560, 14.20693289415472016, -228.8865298551900764 ) ) ;
#3039 = CARTESIAN_POINT ( 'NONE',  ( -9.060295054034883222, 29.20313342278041802, -224.2979742714222482 ) ) ;
#3040 = VERTEX_POINT ( 'NONE', #16620 ) ;
#3041 = CARTESIAN_POINT ( 'NONE',  ( -12.96306772261163154, -8.963621967909368493, -225.1938837381851215 ) ) ;
#3042 = CARTESIAN_POINT ( 'NONE',  ( 16.22460398937575121, -0.7285105026664867589, -219.3274985887512116 ) ) ;
#3043 = TOROIDAL_SURFACE ( 'NONE', #553, 24.63401512838747820, 3.000000000000000888 ) ;
#3044 = FACE_OUTER_BOUND ( 'NONE', #15970, .T. ) ;
#3045 = CARTESIAN_POINT ( 'NONE',  ( -30.56371166594826150, 0.09613004385584933420, -226.3268674980304525 ) ) ;
#3046 = CARTESIAN_POINT ( 'NONE',  ( 10.12956299421491302, 11.38773431477224385, -230.3175791991728829 ) ) ;
#3047 = CARTESIAN_POINT ( 'NONE',  ( -16.88145396433676027, 5.002512658926777434, -221.2364783498041731 ) ) ;
#3048 = CARTESIAN_POINT ( 'NONE',  ( 10.66732316618037402, 25.78610527446713263, -216.5597036843431624 ) ) ;
#3049 = CARTESIAN_POINT ( 'NONE',  ( 13.15438416660314225, 5.520603777723624539, -227.0878346348094681 ) ) ;
#3050 = CARTESIAN_POINT ( 'NONE',  ( -11.17605908769978740, -26.51801958233905765, -230.6004191093659301 ) ) ;
#3051 = EDGE_LOOP ( 'NONE', ( #12162, #17052, #20195, #14283 ) ) ;
#3052 = CARTESIAN_POINT ( 'NONE',  ( -18.96646980336054611, -22.16549408654085696, -227.7928771762007329 ) ) ;
#3053 = CARTESIAN_POINT ( 'NONE',  ( -28.12586305337175219, 12.75764838638491305, -230.3810511299127768 ) ) ;
#3054 = CARTESIAN_POINT ( 'NONE',  ( 14.65870393774896030, -26.09170264574407838, -221.2973805112574723 ) ) ;
#3055 = CARTESIAN_POINT ( 'NONE',  ( -28.46519324992292965, -8.397260794665152517, -225.6705986409035347 ) ) ;
#3056 = TOROIDAL_SURFACE ( 'NONE', #8439, 24.63401512838747820, 3.000000000000000888 ) ;
#3057 = CARTESIAN_POINT ( 'NONE',  ( -14.37894460687751597, -1.926260335694933268, -225.0161641904981593 ) ) ;
#3058 = PRESENTATION_LAYER_ASSIGNMENT (  '', '', ( #9910 ) ) ;
#3059 = CARTESIAN_POINT ( 'NONE',  ( 14.91731358302415877, 13.33846450914490056, -217.2468882285060658 ) ) ;
#3060 = CARTESIAN_POINT ( 'NONE',  ( 0.000000000000000000, 0.000000000000000000, -101.2940952255125922 ) ) ;
#3061 = CARTESIAN_POINT ( 'NONE',  ( -21.75607741976026333, 20.26169853110213381, -228.4128163609909450 ) ) ;
#3062 = CARTESIAN_POINT ( 'NONE',  ( 23.08329078023534109, 11.96623404944238978, -217.1428499060670845 ) ) ;
#3063 = CARTESIAN_POINT ( 'NONE',  ( 18.29617186523616468, 23.20920553663278341, -223.4372550713720216 ) ) ;
#3065 = B_SPLINE_CURVE_WITH_KNOTS ( 'NONE', 3,
 ( #13724, #12032, #22158, #15194, #11810, #4820, #1680, #9899, #6856, #18784, #6971, #16987, #20338, #17208, #101, #15518, #8324, #13843, #11918, #1566, #11697, #8554, #6747, #11577, #3015, #4934, #18566, #8441, #10011, #1451 ),
 .UNSPECIFIED., .F., .F.,
 ( 4, 1, 1, 1, 1, 1, 2, 2, 1, 1, 1, 1, 1, 2, 2, 1, 1, 1, 1, 2, 2, 4 ),
 ( 0.5000000000000000000, 0.5625000000000000000, 0.5937500000000000000, 0.6093750000000001110, 0.6171875000000001110, 0.6210937500000001110, 0.6230468750000001110, 0.6250000000000001110, 0.6875000000000002220, 0.7187500000000003331, 0.7343750000000003331, 0.7421875000000003331, 0.7460937500000003331, 0.7480468750000003331, 0.7500000000000004441, 0.8125000000000004441, 0.8437500000000004441, 0.8593750000000005551, 0.8671875000000005551, 0.8710937500000006661, 0.8750000000000006661, 1.000000000000000000 ),
 .UNSPECIFIED. ) ;
#3064 = CARTESIAN_POINT ( 'NONE',  ( 9.489894741926459432, 25.96007012349547338, -222.3210984495278524 ) ) ;
#3066 = CARTESIAN_POINT ( 'NONE',  ( 13.52447848812844100, -22.07588418332509050, -234.6412735253872484 ) ) ;
#3067 = CARTESIAN_POINT ( 'NONE',  ( -5.529079411693809121, 13.00503897727793401, -226.8014833675713646 ) ) ;
#3068 = DIRECTION ( 'NONE',  ( -1.000000000000000000, 0.000000000000000000, 0.000000000000000000 ) ) ;
#3069 = CARTESIAN_POINT ( 'NONE',  ( 0.000000000000000000, 0.000000000000000000, -24.99999999999999645 ) ) ;
#3070 = CARTESIAN_POINT ( 'NONE',  ( 11.57669841200422134, 10.63052136557218574, -228.9489978335593889 ) ) ;
#3071 = CARTESIAN_POINT ( 'NONE',  ( 6.466495776945791363, -21.72297233841655029, -216.6235280138562302 ) ) ;
#3072 = CARTESIAN_POINT ( 'NONE',  ( -24.39036648059286350, 13.21953970265592027, -220.1632778389106591 ) ) ;
#3073 = EDGE_CURVE ( 'NONE', #2853, #20136, #1755, .T. ) ;
#3074 = PRESENTATION_LAYER_ASSIGNMENT (  '', '', ( #13170 ) ) ;
#3075 = CARTESIAN_POINT ( 'NONE',  ( 8.860681144154234801, 27.11956268701432293, -229.8503778060109823 ) ) ;
#3076 = MECHANICAL_DESIGN_GEOMETRIC_PRESENTATION_REPRESENTATION (  '', ( #21759 ), #15681 ) ;
#3077 = CARTESIAN_POINT ( 'NONE',  ( -16.21268175593173311, -5.852138355245464219, -231.1837890105803410 ) ) ;
#3078 = EDGE_CURVE ( 'NONE', #16621, #14271, #12179, .T. ) ;
#3079 = CARTESIAN_POINT ( 'NONE',  ( -22.10934047915413814, 0.9940043559354462266, -218.9999999999999716 ) ) ;
#3080 = EDGE_CURVE ( 'NONE', #21835, #12695, #14616, .T. ) ;
#3081 = CARTESIAN_POINT ( 'NONE',  ( 15.23494377589453919, 15.24947835004434538, -215.7641128510430519 ) ) ;
#3082 = ORIENTED_EDGE ( 'NONE', *, *, #8473, .T. ) ;
#3083 = CARTESIAN_POINT ( 'NONE',  ( -1.249406995060579062, 25.48934319316224162, -216.9406480707515072 ) ) ;
#3084 = CARTESIAN_POINT ( 'NONE',  ( 23.21483485987735307, -16.21330837850192097, -225.6840547952056397 ) ) ;
#3085 = CARTESIAN_POINT ( 'NONE',  ( 14.46917091355089902, -8.493370822347547033, -231.7163745456035997 ) ) ;
#3086 = LINE ( 'NONE', #14810, #9503 ) ;
#3087 = CARTESIAN_POINT ( 'NONE',  ( 4.559463107227270662, 13.27337529356814017, -226.9596205199204633 ) ) ;
#3088 = CARTESIAN_POINT ( 'NONE',  ( -18.91688971021567767, -12.73417920357403688, -235.2301191595167040 ) ) ;
#3089 = CARTESIAN_POINT ( 'NONE',  ( 5.569356713096689226, -12.06902110579006226, -223.1407905962607003 ) ) ;
#3090 = CARTESIAN_POINT ( 'NONE',  ( 17.15627899979664051, -18.64955541608202694, -217.1729447097152388 ) ) ;
#3091 = CARTESIAN_POINT ( 'NONE',  ( -16.90193019167508126, 18.45790510038867893, -217.5707532411249758 ) ) ;
#3092 = CARTESIAN_POINT ( 'NONE',  ( 12.60818910183731489, 13.02403301690871729, -229.3305689548085695 ) ) ;
#3093 = PLANE ( 'NONE',  #14487 ) ;
#3094 = CARTESIAN_POINT ( 'NONE',  ( -12.27164519775873686, 10.97713184439464840, -231.6269036897678291 ) ) ;
#3095 = CARTESIAN_POINT ( 'NONE',  ( -16.02814206296035593, -12.75525137407698040, -230.7643788161867633 ) ) ;
#3096 = CIRCLE ( 'NONE', #11018, 25.00000000000001066 ) ;
#3097 = ORIENTED_EDGE ( 'NONE', *, *, #16505, .F. ) ;
#3098 = CARTESIAN_POINT ( 'NONE',  ( -5.365396334125453137, 16.47374957271378904, -219.4721119688156534 ) ) ;
#3099 = CARTESIAN_POINT ( 'NONE',  ( 28.03290210476798094, 13.48017620089690638, -224.9212082181537937 ) ) ;
#3100 = CARTESIAN_POINT ( 'NONE',  ( -6.593106361191484410, 26.27107262772703322, -231.8730401762632596 ) ) ;
#3101 = CARTESIAN_POINT ( 'NONE',  ( 11.97732832373273126, -6.576952149368169742, -223.6031523087739572 ) ) ;
#3102 = CARTESIAN_POINT ( 'NONE',  ( 0.000000000000000000, 0.000000000000000000, -120.0000000000000142 ) ) ;
#3103 = VERTEX_POINT ( 'NONE', #11445 ) ;
#3104 = CARTESIAN_POINT ( 'NONE',  ( -9.151299407007059017, 9.196974979111923076, -223.9483834032048719 ) ) ;
#3105 = CARTESIAN_POINT ( 'NONE',  ( -14.03169683822311420, -2.573853926495621725, -218.3324423281324016 ) ) ;
#3106 = CARTESIAN_POINT ( 'NONE',  ( 0.000000000000000000, 0.000000000000000000, -75.00000000000000000 ) ) ;
#3107 = CARTESIAN_POINT ( 'NONE',  ( 11.62313423782632782, 11.98467543564608029, -219.7293303032897995 ) ) ;
#3108 = DIRECTION ( 'NONE',  ( -1.000000000000000000, 0.000000000000000000, -0.000000000000000000 ) ) ;
#3109 = UNCERTAINTY_MEASURE_WITH_UNIT (LENGTH_MEASURE( 1.000000000000000082E-05 ), #15845, 'distance_accuracy_value', 'NONE');
#3110 = CARTESIAN_POINT ( 'NONE',  ( 19.06435866915521515, -20.24829071055443563, -218.8318535520223804 ) ) ;
#3111 =( LENGTH_UNIT ( ) NAMED_UNIT ( * ) SI_UNIT ( .MILLI., .METRE. ) );
#3112 = CARTESIAN_POINT ( 'NONE',  ( -20.54164754914381064, 7.122791156791981493, -233.5720402887671980 ) ) ;
#3113 = PRODUCT_DEFINITION_SHAPE ( 'NONE', 'NONE',  #22271 ) ;
#3114 = CARTESIAN_POINT ( 'NONE',  ( -13.25293905438448405, 17.39325876214774524, -215.6628841494472510 ) ) ;
#3115 = CARTESIAN_POINT ( 'NONE',  ( 28.09488075336259527, 3.911739131332936381, -227.7543364642411632 ) ) ;
#3116 = CARTESIAN_POINT ( 'NONE',  ( -5.139154528335864391, -14.05392405596956529, -226.2842807754188641 ) ) ;
#3117 = CARTESIAN_POINT ( 'NONE',  ( -24.30989004983127799, 5.839958665417457340, -8.124004078861357669 ) ) ;
#3118 = CARTESIAN_POINT ( 'NONE',  ( 16.91879448796214191, 0.8271603773820436212, -230.0510230802265710 ) ) ;
#3119 = CARTESIAN_POINT ( 'NONE',  ( 18.00000000000000000, 1.372269673157290277E-13, -10.00000000000000000 ) ) ;
#3120 = CARTESIAN_POINT ( 'NONE',  ( 15.68576712525985251, -3.705577278900763716, -224.6781181500375908 ) ) ;
#3121 = CARTESIAN_POINT ( 'NONE',  ( -22.51170993270524789, -14.32174306031543054, -231.7292175355062795 ) ) ;
#3122 = LINE ( 'NONE', #18556, #2694 ) ;
#3123 = CARTESIAN_POINT ( 'NONE',  ( 0.000000000000000000, 0.000000000000000000, -70.00000000000000000 ) ) ;
#3124 = CARTESIAN_POINT ( 'NONE',  ( 5.195682580001069084, 14.86321519495278665, -224.7851167466743334 ) ) ;
#3125 = CARTESIAN_POINT ( 'NONE',  ( 11.19883971596842720, -26.43874323075700161, -218.8478122585937626 ) ) ;
#3126 = CARTESIAN_POINT ( 'NONE',  ( 21.05631363308661363, -21.50266115212419393, -222.6654548186096747 ) ) ;
#3127 = CARTESIAN_POINT ( 'NONE',  ( -11.85645341316062051, 18.51497629668490674, -217.8828067666886454 ) ) ;
#3128 = CARTESIAN_POINT ( 'NONE',  ( 12.81769551943392393, 4.437328497131001193, -221.7762769673541072 ) ) ;
#3129 = CARTESIAN_POINT ( 'NONE',  ( 28.52435124311170966, 7.611291969169514005, -224.8315247833735384 ) ) ;
#3130 = CARTESIAN_POINT ( 'NONE',  ( -6.114698591673049854, -22.00309638965383030, -231.6969144128436540 ) ) ;
#3131 = CARTESIAN_POINT ( 'NONE',  ( -14.42982486328545200, 1.701984465643896272, 93.00000000000001421 ) ) ;
#3132 = CARTESIAN_POINT ( 'NONE',  ( -13.91932826323387395, 8.983986115891950064, -216.4624824187541776 ) ) ;
#3133 = CARTESIAN_POINT ( 'NONE',  ( 3.490345297502855715, 11.17751288514984331, -224.7799703251421022 ) ) ;
#3134 = CARTESIAN_POINT ( 'NONE',  ( 9.638496285600583136, -13.08983061985817464, -223.8709389748426588 ) ) ;
#3135 = CARTESIAN_POINT ( 'NONE',  ( 1.217121169770782663, 15.31158828575123110, -230.6845728599757308 ) ) ;
#3136 = CARTESIAN_POINT ( 'NONE',  ( -29.30406754532526037, 5.063969254119831120, -221.8212091093853076 ) ) ;
#3137 = CARTESIAN_POINT ( 'NONE',  ( 18.99256614858759207, 26.22894869843687715, -224.5811130452664202 ) ) ;
#3138 = CARTESIAN_POINT ( 'NONE',  ( -16.75232826114664775, 4.232868982398014346, -229.4158550594996200 ) ) ;
#3139 = CARTESIAN_POINT ( 'NONE',  ( -6.855867220396999251, 12.17758473459128332, -220.6375607554995213 ) ) ;
#3140 = CARTESIAN_POINT ( 'NONE',  ( 0.3188271712753663611, 10.76635261883074257, 92.00000000000001421 ) ) ;
#3141 = CARTESIAN_POINT ( 'NONE',  ( 4.152856881432678726, 16.71326706899027670, -228.3712188091315909 ) ) ;
#3142 = FACE_BOUND ( 'NONE', #22130, .T. ) ;
#3143 = LINE ( 'NONE', #4947, #2344 ) ;
#3144 = DIRECTION ( 'NONE',  ( 1.083936797661038068E-15, 1.000000000000000000, 0.000000000000000000 ) ) ;
#3145 = CARTESIAN_POINT ( 'NONE',  ( -31.76239872120898511, 5.177298019713663990, -226.5714959923072342 ) ) ;
#3146 = CARTESIAN_POINT ( 'NONE',  ( -18.87172488519036762, -12.11125346135639802, -231.2159161446224402 ) ) ;
#3147 = CARTESIAN_POINT ( 'NONE',  ( 19.81239090451986939, 2.079411191919064983, -227.1705409384963161 ) ) ;
#3148 = CARTESIAN_POINT ( 'NONE',  ( -7.375127652145912371, 13.01042140126078195, -223.9959097520547004 ) ) ;
#3149 = CARTESIAN_POINT ( 'NONE',  ( 1.967796959512672306, -15.42100964229427085, -222.1538042820122314 ) ) ;
#3150 = CARTESIAN_POINT ( 'NONE',  ( 16.82251835652528982, 18.18719385133374544, -231.8032941011735772 ) ) ;
#3151 = CARTESIAN_POINT ( 'NONE',  ( -16.84845737324940984, 22.31296517946017488, -228.8910390263689010 ) ) ;
#3152 = CARTESIAN_POINT ( 'NONE',  ( -7.312583518931054627, 16.22063427959223958, -217.3454962955413521 ) ) ;
#3153 = EDGE_LOOP ( 'NONE', ( #14173, #10426, #15370, #5728 ) ) ;
#3154 = CARTESIAN_POINT ( 'NONE',  ( -16.09675311661892039, -3.241155435977624677, -226.6155721728984531 ) ) ;
#3155 = CARTESIAN_POINT ( 'NONE',  ( 7.762960416026701616, 12.60702317161859121, -221.9096828323375235 ) ) ;
#3156 = EDGE_CURVE ( 'NONE', #9492, #8832, #20066, .T. ) ;
#3157 = CARTESIAN_POINT ( 'NONE',  ( -25.11055959288653128, 8.701823109978603199, -230.2231080656787583 ) ) ;
#3158 = CARTESIAN_POINT ( 'NONE',  ( 26.50744623559791435, 1.694095366541529923, -217.6968951254705473 ) ) ;
#3159 = CYLINDRICAL_SURFACE ( 'NONE', #11262, 4.500000000000000888 ) ;
#3160 = CARTESIAN_POINT ( 'NONE',  ( 27.02029988085337919, -0.4174685747284823112, -230.1188858631967378 ) ) ;
#3161 = CARTESIAN_POINT ( 'NONE',  ( 11.96568375430165254, 8.504117401580989721, -219.8633768076029753 ) ) ;
#3162 = CARTESIAN_POINT ( 'NONE',  ( -15.19607346356906952, 9.485739149828241068, -229.2407115334993080 ) ) ;
#3163 = CARTESIAN_POINT ( 'NONE',  ( -3.162425552858488143, 20.40327580806445695, -216.0004724541873316 ) ) ;
#3164 = CARTESIAN_POINT ( 'NONE',  ( 20.02669998934234741, 11.93441252203826508, -216.7824909737982182 ) ) ;
#3165 = CARTESIAN_POINT ( 'NONE',  ( -8.465184826868526358, -8.692222964613778302, -225.5402182279159149 ) ) ;
#3166 = ORIENTED_EDGE ( 'NONE', *, *, #20103, .F. ) ;
#3167 = CARTESIAN_POINT ( 'NONE',  ( -10.30161254035895091, -9.966167094494833734, -223.3409979381218875 ) ) ;
#3168 = AXIS2_PLACEMENT_3D ( 'NONE', #13351, #18422, #4789 ) ;
#3169 = CARTESIAN_POINT ( 'NONE',  ( -12.14471622011552832, 3.716031503296523653, -220.6237729066402835 ) ) ;
#3170 = CARTESIAN_POINT ( 'NONE',  ( 7.088126259304779353, -19.25156530781288566, -233.7785425911077937 ) ) ;
#3171 = CARTESIAN_POINT ( 'NONE',  ( 20.72180063689699026, -9.651256082433341987, -234.7026181832539180 ) ) ;
#3172 = CARTESIAN_POINT ( 'NONE',  ( -14.48876282330270016, -2.056064607042531911, -223.6537127325441361 ) ) ;
#3173 = CARTESIAN_POINT ( 'NONE',  ( 22.22999428328319382, 14.15012104770485557, -232.1858878619060249 ) ) ;
#3174 = CARTESIAN_POINT ( 'NONE',  ( -10.52776196018457711, 13.57482816453351937, -219.2327734183297423 ) ) ;
#3175 = CARTESIAN_POINT ( 'NONE',  ( 22.22999428328319382, 14.15012104770485557, -232.1858878619060249 ) ) ;
#3176 = CARTESIAN_POINT ( 'NONE',  ( 10.07175337281514871, 14.76776740066196325, -231.7834566702614723 ) ) ;
#3177 = CARTESIAN_POINT ( 'NONE',  ( 14.02816775221371337, 20.58276248714641810, -218.7180790146936999 ) ) ;
#3178 = CARTESIAN_POINT ( 'NONE',  ( 21.11934605992122727, -20.14300392389669270, -232.3867613253685249 ) ) ;
#3179 = CARTESIAN_POINT ( 'NONE',  ( -6.255852670334142829, 13.96671599789818252, -220.4426911866496823 ) ) ;
#3180 = DIRECTION ( 'NONE',  ( -0.000000000000000000, -0.000000000000000000, -1.000000000000000000 ) ) ;
#3181 = FACE_OUTER_BOUND ( 'NONE', #7005, .T. ) ;
#3182 = FACE_OUTER_BOUND ( 'NONE', #13047, .T. ) ;
#3183 = CARTESIAN_POINT ( 'NONE',  ( 9.500235314199413139, -15.98409598254677455, -218.3811512014305265 ) ) ;
#3184 = CARTESIAN_POINT ( 'NONE',  ( -14.57944476639264764, 6.129437248167259433, -229.4766146696829310 ) ) ;
#3185 = CARTESIAN_POINT ( 'NONE',  ( 0.8374361358884788720, 23.73768315274483953, -232.4065959030912154 ) ) ;
#3186 = ADVANCED_FACE ( 'NONE', ( #16185 ), #18207, .T. ) ;
#3187 = CARTESIAN_POINT ( 'NONE',  ( -13.72709560065558421, -5.132649126379569715, -227.9317987811764965 ) ) ;
#3188 = CARTESIAN_POINT ( 'NONE',  ( 17.91327661571172314, 1.545939370248587075, -216.9938266089438912 ) ) ;
#3189 = CARTESIAN_POINT ( 'NONE',  ( 9.100443535964535258, 24.01370002727352215, -234.5397711707082635 ) ) ;
#3190 = ORIENTED_EDGE ( 'NONE', *, *, #9938, .T. ) ;
#3191 = CARTESIAN_POINT ( 'NONE',  ( -1.881996891245037995, 28.05344686410985489, -218.6379207300106202 ) ) ;
#3192 = CARTESIAN_POINT ( 'NONE',  ( 12.63976474005154493, -11.16289257830726278, -221.8494566150397134 ) ) ;
#3193 = CARTESIAN_POINT ( 'NONE',  ( 28.81324478616323148, -9.895151559995404966, -227.1624192579662918 ) ) ;
#3194 = DIRECTION ( 'NONE',  ( 1.000000000000000000, 0.000000000000000000, 0.000000000000000000 ) ) ;
#3195 = CARTESIAN_POINT ( 'NONE',  ( 9.586902571418640662, 24.43292817174309661, -231.9968623198229807 ) ) ;
#3196 = CARTESIAN_POINT ( 'NONE',  ( -30.46088052942827318, -8.161173215405806758, -225.9185547777119893 ) ) ;
#3197 = CARTESIAN_POINT ( 'NONE',  ( 0.04660897052267574947, -31.13860575300111577, -224.7746869833732717 ) ) ;
#3198 = CARTESIAN_POINT ( 'NONE',  ( 19.68037530048075112, -17.97179847169212508, -231.8517058357153076 ) ) ;
#3199 = CARTESIAN_POINT ( 'NONE',  ( -22.57344584932824105, 14.14390280519600473, -217.2212543695777924 ) ) ;
#3200 = ADVANCED_FACE ( 'NONE', ( #7633 ), #18989, .F. ) ;
#3201 = CARTESIAN_POINT ( 'NONE',  ( 7.497537106193371770, 19.52448593130572618, -231.1338690134634248 ) ) ;
#3202 = CARTESIAN_POINT ( 'NONE',  ( -15.48255455842386219, 10.01793346089237069, -233.1197357361336913 ) ) ;
#3203 = CARTESIAN_POINT ( 'NONE',  ( -20.76981451797363576, 10.27702766794165257, -234.3988437453480742 ) ) ;
#3204 = CARTESIAN_POINT ( 'NONE',  ( -14.26213125333782727, -4.747741064748048245, -225.2154851558723294 ) ) ;
#3205 = VERTEX_POINT ( 'NONE', #16292 ) ;
#3206 = CARTESIAN_POINT ( 'NONE',  ( -10.40174557315337900, 22.75579539577861965, -231.4492192189165962 ) ) ;
#3207 = CARTESIAN_POINT ( 'NONE',  ( 14.50618777373884960, 4.375057440872940795, -230.8807389798650433 ) ) ;
#3208 = CARTESIAN_POINT ( 'NONE',  ( 5.179557175392591972, 10.46258103618983881, -224.6216839350439614 ) ) ;
#3209 = CARTESIAN_POINT ( 'NONE',  ( 26.86480837698434243, -8.606671353193281249, -231.2046318962545683 ) ) ;
#3210 = CARTESIAN_POINT ( 'NONE',  ( 0.000000000000000000, 19.80000000000006111, 78.50000000000000000 ) ) ;
#3211 = ORIENTED_EDGE ( 'NONE', *, *, #4968, .T. ) ;
#3212 = CARTESIAN_POINT ( 'NONE',  ( -23.98802705797876200, 19.46654170242919690, -223.5293093576406989 ) ) ;
#3213 = CARTESIAN_POINT ( 'NONE',  ( -29.95626564321166541, -9.027512590954497540, -220.3228832733970819 ) ) ;
#3214 = DIRECTION ( 'NONE',  ( 1.000000000000000000, 0.000000000000000000, 0.000000000000000000 ) ) ;
#3215 = CARTESIAN_POINT ( 'NONE',  ( 10.78187269046063435, 10.73871010366167944, -221.9206544238666368 ) ) ;
#3216 = DIRECTION ( 'NONE',  ( -1.000000000000000000, 0.000000000000000000, 0.000000000000000000 ) ) ;
#3217 = CARTESIAN_POINT ( 'NONE',  ( 15.54083024098960486, -10.44392130763852222, -217.6620978190037476 ) ) ;
#3218 = CARTESIAN_POINT ( 'NONE',  ( -29.95012366401462955, 4.746560250930182967, -224.6954343660969471 ) ) ;
#3219 = CARTESIAN_POINT ( 'NONE',  ( -8.329232059016652201, 11.81357365351366617, -230.1839637212758021 ) ) ;
#3220 = CARTESIAN_POINT ( 'NONE',  ( 28.56567312134318826, 3.451746495494312672, -224.1550573921799412 ) ) ;
#3221 = CARTESIAN_POINT ( 'NONE',  ( -4.902442737337177725, -13.94343087703807704, -224.3742458082145959 ) ) ;
#3222 = DIRECTION ( 'NONE',  ( -1.000000000000000000, 0.000000000000000000, 0.000000000000000000 ) ) ;
#3223 = CARTESIAN_POINT ( 'NONE',  ( 15.05360126642391450, 1.481754003466396963, -222.9454997252120734 ) ) ;
#3224 = DIRECTION ( 'NONE',  ( -1.000000000000000000, 0.000000000000000000, 0.000000000000000000 ) ) ;
#3225 = CARTESIAN_POINT ( 'NONE',  ( 11.76368234164141136, -12.26645877504561888, -220.6132173800162946 ) ) ;
#3226 = CARTESIAN_POINT ( 'NONE',  ( 12.88473959921682166, -2.638886110283121589, -223.5604664187585229 ) ) ;
#3227 = CARTESIAN_POINT ( 'NONE',  ( -22.77702959565148788, -3.252406101723253062, 9.478689975477541552 ) ) ;
#3228 = CARTESIAN_POINT ( 'NONE',  ( 6.332229114051408203, 16.75791367489523154, -229.7702805136205200 ) ) ;
#3229 = CARTESIAN_POINT ( 'NONE',  ( 5.646952844456516019, 23.06006924884521325, -218.8221376988549878 ) ) ;
#3230 = CARTESIAN_POINT ( 'NONE',  ( 16.60513614482655598, -17.51558294309126396, -234.8138649271977556 ) ) ;
#3231 = CARTESIAN_POINT ( 'NONE',  ( 13.47054497134856277, -24.75371201277411615, -218.7687119198782000 ) ) ;
#3232 = ORIENTED_EDGE ( 'NONE', *, *, #6382, .F. ) ;
#3233 = CARTESIAN_POINT ( 'NONE',  ( -16.84845737324940984, 22.31296517946017488, -228.8910390263689010 ) ) ;
#3234 = CARTESIAN_POINT ( 'NONE',  ( 22.42925200799500729, 5.652256920629083581, -234.0734181799116698 ) ) ;
#3235 = CARTESIAN_POINT ( 'NONE',  ( 24.38255093784924199, 7.851200578213498815, -231.2687759850219607 ) ) ;
#3236 = VERTEX_POINT ( 'NONE', #21228 ) ;
#3237 = CARTESIAN_POINT ( 'NONE',  ( -3.190684129821126813, -24.11035010539542611, -218.3286195476113392 ) ) ;
#3238 = LINE ( 'NONE', #3467, #7997 ) ;
#3239 = CARTESIAN_POINT ( 'NONE',  ( -13.00859847561873117, 4.399982435993697649, -231.0885370824921097 ) ) ;
#3240 = VERTEX_POINT ( 'NONE', #4340 ) ;
#3241 = CARTESIAN_POINT ( 'NONE',  ( 14.65697969206133067, 11.40587726087447606, -233.3943609825344652 ) ) ;
#3242 = CARTESIAN_POINT ( 'NONE',  ( 11.33829581046623858, -17.80819325066959635, -230.7883484307220385 ) ) ;
#3243 = CARTESIAN_POINT ( 'NONE',  ( 7.995304978256253747, 13.28024228361502779, -220.6535174700288451 ) ) ;
#3244 = CARTESIAN_POINT ( 'NONE',  ( -27.82842955277035202, 11.70195273568964112, -227.9294339757464911 ) ) ;
#3245 = CARTESIAN_POINT ( 'NONE',  ( 8.373295497769937867, 8.203271496719947820, -226.1884629658694053 ) ) ;
#3246 = CARTESIAN_POINT ( 'NONE',  ( -13.43384090552117271, 6.057765724406720231, -225.7182623230366119 ) ) ;
#3247 = CARTESIAN_POINT ( 'NONE',  ( -9.740348021262962064, 16.12529029871877384, -216.4361617420699702 ) ) ;
#3248 = CARTESIAN_POINT ( 'NONE',  ( 15.05360126642391450, 1.481754003466396963, -222.9454997252120734 ) ) ;
#3249 = CARTESIAN_POINT ( 'NONE',  ( 8.115778909262310492, -29.92983049028717346, -224.5060555478150377 ) ) ;
#3250 = FACE_OUTER_BOUND ( 'NONE', #12502, .T. ) ;
#3251 = CARTESIAN_POINT ( 'NONE',  ( 1.665334536937734811E-13, -23.00000000000000000, -69.99999999999998579 ) ) ;
#3252 = EDGE_CURVE ( 'NONE', #12810, #12003, #3901, .T. ) ;
#3253 = CARTESIAN_POINT ( 'NONE',  ( -14.48876282330270016, -2.056064607042531911, -223.6537127325441361 ) ) ;
#3254 = CARTESIAN_POINT ( 'NONE',  ( -20.02994071726468661, 1.326980477106467271, -234.9527056834518532 ) ) ;
#3255 = CARTESIAN_POINT ( 'NONE',  ( -20.29356827505781879, -18.19569389227462253, -221.0297756488607490 ) ) ;
#3256 = DIRECTION ( 'NONE',  ( -1.000000000000000000, 0.000000000000000000, 0.000000000000000000 ) ) ;
#3257 = FILL_AREA_STYLE ('',( #6873 ) ) ;
#3258 = CARTESIAN_POINT ( 'NONE',  ( 5.625090746907006611, -14.93184515622287201, -221.0486942310484721 ) ) ;
#3259 = CARTESIAN_POINT ( 'NONE',  ( 11.41090957555148222, 16.52772439454343711, -218.2458222691329013 ) ) ;
#3260 = CARTESIAN_POINT ( 'NONE',  ( -13.51991436508781597, 16.61129329384914755, -232.1184346153593197 ) ) ;
#3261 = CARTESIAN_POINT ( 'NONE',  ( -16.89013823391154290, 26.38860451648245231, -225.6449744083545852 ) ) ;
#3262 = ORIENTED_EDGE ( 'NONE', *, *, #4428, .F. ) ;
#3263 = CARTESIAN_POINT ( 'NONE',  ( 28.26377063890550190, -1.722554810693586180, -217.1290174754948623 ) ) ;
#3264 = EDGE_LOOP ( 'NONE', ( #19648, #10645 ) ) ;
#3265 = CARTESIAN_POINT ( 'NONE',  ( 10.57926812561479757, 10.00910231482511215, -225.8341706491384286 ) ) ;
#3266 = CARTESIAN_POINT ( 'NONE',  ( -22.32700334442577272, 3.978587747811427988, -218.4803616146862453 ) ) ;
#3267 = CARTESIAN_POINT ( 'NONE',  ( 30.57915561709945251, 3.468229287067555067, -223.8876084027091906 ) ) ;
#3268 = DIRECTION ( 'NONE',  ( 0.000000000000000000, 0.000000000000000000, -1.000000000000000000 ) ) ;
#3269 = CARTESIAN_POINT ( 'NONE',  ( 12.96449997971774870, 8.285709878278680662, -230.9518598506670628 ) ) ;
#3270 = CARTESIAN_POINT ( 'NONE',  ( -27.32939371162572684, 5.861081283609568260, -224.9659309793921409 ) ) ;
#3271 = CARTESIAN_POINT ( 'NONE',  ( 6.523529190399725231, 13.69551997595937465, -217.3678933099786832 ) ) ;
#3272 = CARTESIAN_POINT ( 'NONE',  ( 21.14328650935969023, 6.072767611243683916, -217.6422864096696514 ) ) ;
#3273 = CARTESIAN_POINT ( 'NONE',  ( -7.835169104947472540, -15.11139199849201908, -217.2594261031170220 ) ) ;
#3274 = EDGE_LOOP ( 'NONE', ( #3082, #777, #2298, #22194 ) ) ;
#3275 = CARTESIAN_POINT ( 'NONE',  ( -19.65071121466273496, -22.30814805266854606, -225.1308016072272267 ) ) ;
#3276 = ADVANCED_FACE ( 'NONE', ( #5013 ), #15389, .F. ) ;
#3277 = CARTESIAN_POINT ( 'NONE',  ( -20.87212828950092813, -0.8819659211619411687, -215.0000000018925448 ) ) ;
#3278 = CARTESIAN_POINT ( 'NONE',  ( 8.021672912688133650, -23.92397517040199872, -233.3380040120402441 ) ) ;
#3279 = CARTESIAN_POINT ( 'NONE',  ( -2.735889804569492600, 12.71735652435744512, -225.1194195722198117 ) ) ;
#3280 = CARTESIAN_POINT ( 'NONE',  ( 12.01003603113874441, -9.270215614621081457, -232.3219482526175170 ) ) ;
#3281 = CARTESIAN_POINT ( 'NONE',  ( -18.11268275035277853, -3.459088653808292335, -218.4233329573673359 ) ) ;
#3282 = CARTESIAN_POINT ( 'NONE',  ( 13.71882454279727526, 6.278400000045776252, -230.2269611870541723 ) ) ;
#3283 = DIRECTION ( 'NONE',  ( 0.000000000000000000, 0.000000000000000000, -1.000000000000000000 ) ) ;
#3284 = CARTESIAN_POINT ( 'NONE',  ( -17.07051451008491938, 15.19890664381897949, -233.6014043774825666 ) ) ;
#3285 = CARTESIAN_POINT ( 'NONE',  ( 11.83256327006771969, 5.988634687709346593, -225.8999299265561831 ) ) ;
#3286 = CIRCLE ( 'NONE', #10846, 10.76794919243112325 ) ;
#3287 = CARTESIAN_POINT ( 'NONE',  ( 12.23063869552301242, 12.84118223717021934, -218.8273164334868284 ) ) ;
#3288 = CARTESIAN_POINT ( 'NONE',  ( 6.402706778685327116, 14.41397785959879307, -226.0127495172349086 ) ) ;
#3289 = CARTESIAN_POINT ( 'NONE',  ( -3.642659482353215239, -13.10753628101701018, -222.6432544668793980 ) ) ;
#3290 = CARTESIAN_POINT ( 'NONE',  ( -6.804439720554941395, 15.25609613835249156, -218.7834354895107651 ) ) ;
#3291 = CARTESIAN_POINT ( 'NONE',  ( 18.46552355142154411, 5.019711608606525211, -231.5099115070375433 ) ) ;
#3292 = CARTESIAN_POINT ( 'NONE',  ( 8.958604797576050771, -20.52636309154128114, -232.6441826665315205 ) ) ;
#3293 = CARTESIAN_POINT ( 'NONE',  ( -22.38347148959098121, 12.58966534755613687, -218.4978713241202399 ) ) ;
#3294 = CARTESIAN_POINT ( 'NONE',  ( -4.583529401292260275, 28.77615850237956607, -226.7744741901706504 ) ) ;
#3295 = CARTESIAN_POINT ( 'NONE',  ( -19.50907964299920039, -17.77536300509877876, -217.8007844881196320 ) ) ;
#3296 = CARTESIAN_POINT ( 'NONE',  ( 20.13946171159960841, -0.1427001808266660232, -233.7987036390019853 ) ) ;
#3297 = AXIS2_PLACEMENT_3D ( 'NONE', #20564, #22039, #15310 ) ;
#3298 = CARTESIAN_POINT ( 'NONE',  ( 10.82528077991200810, 8.849546035972329250, -221.2068619981234008 ) ) ;
#3299 = ORIENTED_EDGE ( 'NONE', *, *, #14893, .F. ) ;
#3300 = CARTESIAN_POINT ( 'NONE',  ( -2.735889804569492600, 12.71735652435744512, -225.1194195722198117 ) ) ;
#3301 = CARTESIAN_POINT ( 'NONE',  ( 16.50219604690516206, -6.005650786285340104, -230.9082164827931933 ) ) ;
#3302 = CARTESIAN_POINT ( 'NONE',  ( 14.79879825009101069, -3.130997509566451953, -219.4569190381675696 ) ) ;
#3303 = EDGE_CURVE ( 'NONE', #10528, #14639, #18751, .T. ) ;
#3304 = FACE_OUTER_BOUND ( 'NONE', #10785, .T. ) ;
#3305 = CARTESIAN_POINT ( 'NONE',  ( -3.855805549595750392, 26.68244055262801950, -232.4569730455296508 ) ) ;
#3306 = CARTESIAN_POINT ( 'NONE',  ( -27.49927005802855717, -8.180762508579555004, -232.0193187950690970 ) ) ;
#3307 = CARTESIAN_POINT ( 'NONE',  ( -15.48425879135615446, -25.29886615046042309, -220.6886037686364261 ) ) ;
#3308 = CARTESIAN_POINT ( 'NONE',  ( 13.99926435381047618, -21.11851526759364006, -232.9234173943665951 ) ) ;
#3309 = CARTESIAN_POINT ( 'NONE',  ( -11.07173923371951574, 9.938770595667456575, -229.9381419817434562 ) ) ;
#3310 = CARTESIAN_POINT ( 'NONE',  ( 17.35243190875273811, 16.67741344734974263, -230.5744436858935558 ) ) ;
#3311 = CARTESIAN_POINT ( 'NONE',  ( -18.08305592660031991, 4.022743421239192152, -217.2335041149100050 ) ) ;
#3312 = CARTESIAN_POINT ( 'NONE',  ( -11.07173923371951574, 9.938770595667456575, -229.9381419817434562 ) ) ;
#3313 = CARTESIAN_POINT ( 'NONE',  ( -12.03049011398204726, -11.12540611457240480, -223.2385418847515268 ) ) ;
#3314 = AXIS2_PLACEMENT_3D ( 'NONE', #1193, #18305, #11216 ) ;
#3315 = ADVANCED_FACE ( 'NONE', ( #5120 ), #6783, .T. ) ;
#3316 = AXIS2_PLACEMENT_3D ( 'NONE', #1464, #11824, #18690 ) ;
#3317 = CARTESIAN_POINT ( 'NONE',  ( -6.720912670637915198, 19.69156892798266512, -217.8848069150180891 ) ) ;
#3318 = CARTESIAN_POINT ( 'NONE',  ( 28.65393683769942967, 4.398063292302325067, -219.1542358361629965 ) ) ;
#3319 = CARTESIAN_POINT ( 'NONE',  ( 11.50837930502119733, 10.86662242793286381, -233.1728506169798436 ) ) ;
#3320 = CARTESIAN_POINT ( 'NONE',  ( 12.31594623278127720, -7.047777776961618557, -228.0736214755532956 ) ) ;
#3321 = CARTESIAN_POINT ( 'NONE',  ( 26.00000000000000000, -3.600000000000001421, -2.699999999999999289 ) ) ;
#3322 = ORIENTED_EDGE ( 'NONE', *, *, #12216, .F. ) ;
#3323 = CARTESIAN_POINT ( 'NONE',  ( -3.514547081416551588, 30.38636916157537016, -227.3529586180979436 ) ) ;
#3324 = CARTESIAN_POINT ( 'NONE',  ( -22.78031074599627814, -9.151179398885634697, -235.0532497368941733 ) ) ;
#3325 = CARTESIAN_POINT ( 'NONE',  ( 0.000000000000000000, 0.000000000000000000, 77.51594804401857175 ) ) ;
#3326 = CARTESIAN_POINT ( 'NONE',  ( 26.48990917286906921, 12.16675355942207659, -225.0153622588060216 ) ) ;
#3327 = CARTESIAN_POINT ( 'NONE',  ( -18.46722752239034193, 0.9784074152395518809, -232.1633353206286188 ) ) ;
#3328 = CARTESIAN_POINT ( 'NONE',  ( 21.05631363308661363, -21.50266115212419393, -222.6654548186096747 ) ) ;
#3329 = CARTESIAN_POINT ( 'NONE',  ( -26.02440924314744919, 2.824604386891162111, -232.0644005296583430 ) ) ;
#3330 = TOROIDAL_SURFACE ( 'NONE', #6934, 24.63401512838747820, 3.000000000000000888 ) ;
#3331 = CARTESIAN_POINT ( 'NONE',  ( 24.60354977307301283, 7.993510024274534942, -218.5358880819990759 ) ) ;
#3332 = CARTESIAN_POINT ( 'NONE',  ( 1.250172743705837641, -19.35180105203422940, -231.6553945523530729 ) ) ;
#3333 = CIRCLE ( 'NONE', #20207, 23.00000000000008882 ) ;
#3334 = DIRECTION ( 'NONE',  ( 1.224646799147353207E-16, 1.000000000000000000, -0.000000000000000000 ) ) ;
#3335 = CARTESIAN_POINT ( 'NONE',  ( 15.42212722119060864, 5.401662248084913465, -220.8333402320903645 ) ) ;
#3336 = CARTESIAN_POINT ( 'NONE',  ( -16.15126510923403202, -0.4755054218165427615, -219.3066569788202571 ) ) ;
#3337 = CARTESIAN_POINT ( 'NONE',  ( 15.80653577316150837, -24.09293983082412893, -226.7583346419201575 ) ) ;
#3338 = CARTESIAN_POINT ( 'NONE',  ( 14.80787930410854081, -2.237450434840648761, -227.0005678990481215 ) ) ;
#3339 = CARTESIAN_POINT ( 'NONE',  ( 19.81538647100171957, -2.076704763782542429, -227.1730004250662773 ) ) ;
#3340 = CARTESIAN_POINT ( 'NONE',  ( 8.647507700742417924, 16.42978512283924175, -220.3082116258600536 ) ) ;
#3341 = CARTESIAN_POINT ( 'NONE',  ( 10.01015180241662605, 20.19019600914695900, -219.1042218506083543 ) ) ;
#3342 = CARTESIAN_POINT ( 'NONE',  ( 11.05135090310477786, -21.04892152267781569, -234.3520113253972568 ) ) ;
#3343 = CARTESIAN_POINT ( 'NONE',  ( 9.584731462935641488, -12.36622837314704348, -230.4796538097028531 ) ) ;
#3344 = ORIENTED_EDGE ( 'NONE', *, *, #12459, .T. ) ;
#3345 = CARTESIAN_POINT ( 'NONE',  ( -8.611121136347097860, 17.46802294375265419, -231.5575697815534113 ) ) ;
#3346 = CARTESIAN_POINT ( 'NONE',  ( -14.47418542577149836, 8.806675964858893479, -228.0010566307936699 ) ) ;
#3347 = CARTESIAN_POINT ( 'NONE',  ( 17.02590609996173754, 6.796709046606974169, -230.8496778635019098 ) ) ;
#3348 = ORIENTED_EDGE ( 'NONE', *, *, #13732, .T. ) ;
#3349 = CARTESIAN_POINT ( 'NONE',  ( -5.110696651857618455, -18.61886646437566384, -231.2604145522360000 ) ) ;
#3350 = DIRECTION ( 'NONE',  ( 0.000000000000000000, 0.000000000000000000, -1.000000000000000000 ) ) ;
#3351 = AXIS2_PLACEMENT_3D ( 'NONE', #14118, #5542, #19272 ) ;
#3352 = ORIENTED_EDGE ( 'NONE', *, *, #2399, .T. ) ;
#3353 = CIRCLE ( 'NONE', #18101, 17.50000000000000711 ) ;
#3354 = CARTESIAN_POINT ( 'NONE',  ( 23.04342321161690776, 14.90264581583150694, -218.4777833225197412 ) ) ;
#3355 = CARTESIAN_POINT ( 'NONE',  ( 13.80508996112396680, -23.93364289317450400, -226.6703843709330783 ) ) ;
#3356 = CARTESIAN_POINT ( 'NONE',  ( 10.85888002857596923, 15.81835858589122878, -232.3913150909872627 ) ) ;
#3357 = CARTESIAN_POINT ( 'NONE',  ( -17.75316132689678383, 25.03468689048078843, -222.1645193425721061 ) ) ;
#3358 = EDGE_CURVE ( 'NONE', #20674, #9897, #2801, .T. ) ;
#3359 = CARTESIAN_POINT ( 'NONE',  ( 5.964915545484365644, 11.50358694729900577, -229.9646467236423462 ) ) ;
#3360 = CARTESIAN_POINT ( 'NONE',  ( -19.27153818831731158, 23.75761453444584248, -221.9111479746408975 ) ) ;
#3361 = EDGE_CURVE ( 'NONE', #6741, #945, #20046, .T. ) ;
#3362 = CARTESIAN_POINT ( 'NONE',  ( 0.4042326456706432647, 15.50845657815858303, -219.2680337625893401 ) ) ;
#3363 = CARTESIAN_POINT ( 'NONE',  ( 21.60524407607017849, 3.028118258437591415, -217.8361640396714449 ) ) ;
#3364 = AXIS2_PLACEMENT_3D ( 'NONE', #18542, #13356, #13475 ) ;
#3365 = CARTESIAN_POINT ( 'NONE',  ( 7.437838793555467731, -20.85539581353325289, -233.9154700400843865 ) ) ;
#3366 = CARTESIAN_POINT ( 'NONE',  ( 24.59129902578158067, -8.191391589517788674, -218.4338547727923299 ) ) ;
#3367 = DIRECTION ( 'NONE',  ( -0.000000000000000000, -0.000000000000000000, -1.000000000000000000 ) ) ;
#3368 = CARTESIAN_POINT ( 'NONE',  ( -15.15819830826754355, -2.370657588173597841, -221.8013720140894236 ) ) ;
#3369 = CARTESIAN_POINT ( 'NONE',  ( -13.63292518690856170, 3.968236334994402981, -218.3158317831635316 ) ) ;
#3370 = CARTESIAN_POINT ( 'NONE',  ( -10.64756522805915395, -11.91724881161430361, -221.7317784521105750 ) ) ;
#3371 = PRESENTATION_STYLE_ASSIGNMENT (( #21940 ) ) ;
#3372 = CARTESIAN_POINT ( 'NONE',  ( 13.65368867897269389, -25.84127502057983605, -227.3223880387346867 ) ) ;
#3373 = CARTESIAN_POINT ( 'NONE',  ( -24.15814485343234352, 4.373587128574028426, -232.6698675874553430 ) ) ;
#3374 = CARTESIAN_POINT ( 'NONE',  ( 3.846342036506673612, 16.55327908958690131, -231.1358846258000597 ) ) ;
#3375 = CARTESIAN_POINT ( 'NONE',  ( -4.558896566524145655, 13.01459016691503301, -228.3167740496058684 ) ) ;
#3376 = ORIENTED_EDGE ( 'NONE', *, *, #11036, .T. ) ;
#3377 = CARTESIAN_POINT ( 'NONE',  ( 22.16968511661848495, 1.542591969257128826, -234.6098499860488857 ) ) ;
#3378 = ORIENTED_EDGE ( 'NONE', *, *, #14496, .F. ) ;
#3379 = CARTESIAN_POINT ( 'NONE',  ( 10.50530447320976535, 20.19629329636330084, -217.1354359361034767 ) ) ;
#3380 = CARTESIAN_POINT ( 'NONE',  ( -21.28804099221702018, -0.9277163183344186992, -219.0000000002572733 ) ) ;
#3381 = CARTESIAN_POINT ( 'NONE',  ( -19.92987771446595957, 11.92619342620000999, -232.5382020162021206 ) ) ;
#3382 = CARTESIAN_POINT ( 'NONE',  ( -14.03072379416114757, -18.13329758221107824, -232.5220584501505812 ) ) ;
#3383 = CARTESIAN_POINT ( 'NONE',  ( 0.000000000000000000, -23.00000000000006040, 75.00000000000000000 ) ) ;
#3384 = APPLICATION_CONTEXT ( 'automotive_design' ) ;
#3385 = DIRECTION ( 'NONE',  ( 0.000000000000000000, 0.000000000000000000, -1.000000000000000000 ) ) ;
#3386 = COLOUR_RGB ( '', 0.31764706, 0.68627451, 0.89019608) ;
#3387 = CARTESIAN_POINT ( 'NONE',  ( -18.33565906012873725, 9.491905303418088025, -219.1855745749628568 ) ) ;
#3388 = CARTESIAN_POINT ( 'NONE',  ( 2.892356176081334773, 24.03953794589038395, -215.3901262983647200 ) ) ;
#3389 = CARTESIAN_POINT ( 'NONE',  ( 11.41911493375616260, 8.796695304819765582, -229.7440655656592412 ) ) ;
#3390 = CARTESIAN_POINT ( 'NONE',  ( -3.174954051807135080, -13.80109495427747746, -226.5796556275459750 ) ) ;
#3391 = VERTEX_POINT ( 'NONE', #3321 ) ;
#3392 = CARTESIAN_POINT ( 'NONE',  ( -8.465333986790207987, -12.59497810381903982, -228.1424919783533198 ) ) ;
#3393 = CARTESIAN_POINT ( 'NONE',  ( -16.96626096607909417, 26.06638125783293347, -227.3272535207661349 ) ) ;
#3394 = CARTESIAN_POINT ( 'NONE',  ( 10.40291689048662782, -13.87512507945592333, -231.9656913702303029 ) ) ;
#3395 = CARTESIAN_POINT ( 'NONE',  ( 0.9046320824004248085, 13.39785254849979701, -226.4815711199935890 ) ) ;
#3396 = CARTESIAN_POINT ( 'NONE',  ( 10.56186985702850833, -7.684747726859879613, -229.4341029534429026 ) ) ;
#3397 = CARTESIAN_POINT ( 'NONE',  ( -13.22951852716680676, -5.246159916193459338, -223.7538483380451453 ) ) ;
#3398 = CARTESIAN_POINT ( 'NONE',  ( -20.45797657813638182, 1.164962349958370336, -217.1306074022350572 ) ) ;
#3399 = CARTESIAN_POINT ( 'NONE',  ( 0.000000000000000000, 23.00000000000006040, -55.00000000000000711 ) ) ;
#3400 = PRODUCT_RELATED_PRODUCT_CATEGORY ( 'part', '', ( #13558 ) ) ;
#3401 = CARTESIAN_POINT ( 'NONE',  ( -8.115738378024497379, 16.90402287339461296, -219.0833473190803034 ) ) ;
#3402 = CARTESIAN_POINT ( 'NONE',  ( 18.75523091462765990, 19.46592657336209697, -230.4909883316157391 ) ) ;
#3403 = VECTOR ( 'NONE', #6983, 1000.000000000000000 ) ;
#3404 = CARTESIAN_POINT ( 'NONE',  ( 14.95414693437772868, 8.262206471704862665, -230.1862972580043163 ) ) ;
#3405 = CARTESIAN_POINT ( 'NONE',  ( 20.47387447818710271, 7.390772095927000684, -234.0991886097562258 ) ) ;
#3406 = CARTESIAN_POINT ( 'NONE',  ( -0.8305687497496098137, -27.95880702065288759, -232.3543905114424888 ) ) ;
#3407 = B_SPLINE_CURVE_WITH_KNOTS ( 'NONE', 3,
 ( #11239, #12824, #19667, #16422, #2677, #7649, #16525, #19885, #9338, #18223, #1104, #14844, #21687, #16198, #6278, #4254, #6500, #3455, #4924, #1668, #12021, #10222, #18441, #8543, #1555, #13488, #6388, #5139, #10334, #21911, #22252, #11684, #6845, #8203, #14961, #22027, #6736, #11800, #1219, #21801, #8094, #1331, #11906, #3227, #20551, #6618, #16975, #13260 ),
 .UNSPECIFIED., .F., .F.,
 ( 4, 2, 2, 2, 2, 2, 2, 2, 2, 2, 2, 2, 2, 2, 2, 2, 2, 2, 2, 2, 2, 2, 2, 4 ),
 ( 1.201007004285936770E-19, 0.001979062126186861923, 0.002968593189280293101, 0.003958124252373724714, 0.005937186378560591407, 0.006926717441654025621, 0.007916248504747461570, 0.008905779567840894917, 0.009895310630934329998, 0.01187437275712120190, 0.01286390382021463698, 0.01385343488330807553, 0.01583249700949494396, 0.01682202807258837904, 0.01781155913568181065, 0.01880109019877524573, 0.01979062126186868081, 0.02176968338805555098, 0.02374874551424242461, 0.02572780764042929824, 0.02671733870352273679, 0.02770686976661617534, 0.02968593189280304898, 0.03166499401898992955 ),
 .UNSPECIFIED. ) ;
#3408 = CARTESIAN_POINT ( 'NONE',  ( -6.094651895680649467, 13.59752566126439177, -221.0608041154719103 ) ) ;
#3409 = CARTESIAN_POINT ( 'NONE',  ( 16.64225601860865211, 1.926018578292457928, -220.2177910260893725 ) ) ;
#3410 = CARTESIAN_POINT ( 'NONE',  ( 2.697602325873029727, -29.85947730167685421, -229.1126320946688111 ) ) ;
#3411 = CARTESIAN_POINT ( 'NONE',  ( -22.13857085231108712, 6.545953331035805789, -217.2801712530867633 ) ) ;
#3412 = CARTESIAN_POINT ( 'NONE',  ( -0.5888410438786807477, 14.99789765555501475, -227.7044550383138244 ) ) ;
#3413 = CARTESIAN_POINT ( 'NONE',  ( -28.46519324992292965, -8.397260794665152517, -225.6705986409035347 ) ) ;
#3414 = CARTESIAN_POINT ( 'NONE',  ( 14.46993441875745390, 0.2699826811589002284, -230.0986938382904157 ) ) ;
#3416 = CARTESIAN_POINT ( 'NONE',  ( 17.81160404892403193, 9.939217752910943560, -216.9646549374535311 ) ) ;
#3415 = AXIS2_PLACEMENT_3D ( 'NONE', #4146, #4584, #9560 ) ;
#3417 = ORIENTED_EDGE ( 'NONE', *, *, #12728, .T. ) ;
#3418 = CARTESIAN_POINT ( 'NONE',  ( 7.762960416026701616, 12.60702317161859121, -221.9096828323375235 ) ) ;
#3419 = CARTESIAN_POINT ( 'NONE',  ( 15.40548389857710987, -8.435137368586953954, -220.3367290259554920 ) ) ;
#3420 = CIRCLE ( 'NONE', #1632, 1.000000000000000888 ) ;
#3421 = CARTESIAN_POINT ( 'NONE',  ( 12.44471834243122466, -10.90083019301730083, -219.2211511521849161 ) ) ;
#3422 = CARTESIAN_POINT ( 'NONE',  ( 11.62313423782632782, 11.98467543564608029, -219.7293303032897995 ) ) ;
#3423 = CARTESIAN_POINT ( 'NONE',  ( -16.38285517717123341, -14.67507636997927989, -214.6561055496966901 ) ) ;
#3424 = CARTESIAN_POINT ( 'NONE',  ( -1.308474130992312023, -24.58654860180777391, -216.2430112183533026 ) ) ;
#3425 = CARTESIAN_POINT ( 'NONE',  ( 9.358654279681809740, -11.94480763145079472, -229.8864256833185777 ) ) ;
#3426 = CARTESIAN_POINT ( 'NONE',  ( -21.12280458060320498, 13.61074013710079988, -216.5529903464332335 ) ) ;
#3427 = CARTESIAN_POINT ( 'NONE',  ( 8.856360819293511710, 14.24139612884802553, -227.7731680686805475 ) ) ;
#3428 = CARTESIAN_POINT ( 'NONE',  ( -15.82069055112642353, 8.315535108674763976, -217.2800172218543935 ) ) ;
#3429 = CARTESIAN_POINT ( 'NONE',  ( -7.366083718505351818, 19.86648438590005838, -231.8662444779758971 ) ) ;
#3430 = CARTESIAN_POINT ( 'NONE',  ( 27.76845665997775114, -9.103683020204879739, -229.9743915588940979 ) ) ;
#3431 = VERTEX_POINT ( 'NONE', #9869 ) ;
#3432 = CARTESIAN_POINT ( 'NONE',  ( -16.84845737324940984, 22.31296517946017488, -228.8910390263689010 ) ) ;
#3433 = CARTESIAN_POINT ( 'NONE',  ( 22.20554449732931346, 18.01468431515759860, -218.9348803756412849 ) ) ;
#3434 = CARTESIAN_POINT ( 'NONE',  ( 6.523529190399725231, 13.69551997595937465, -217.3678933099786832 ) ) ;
#3435 = CARTESIAN_POINT ( 'NONE',  ( 13.66436340482409761, -13.84785698770488871, -232.6553000701566134 ) ) ;
#3436 = DIRECTION ( 'NONE',  ( -1.000000000000000000, -0.000000000000000000, -0.000000000000000000 ) ) ;
#3437 = ORIENTED_EDGE ( 'NONE', *, *, #20358, .F. ) ;
#3438 = MECHANICAL_DESIGN_GEOMETRIC_PRESENTATION_REPRESENTATION (  '', ( #17109 ), #9213 ) ;
#3439 = CARTESIAN_POINT ( 'NONE',  ( -10.84997096467605182, 25.01800101807719301, -232.4518260228253155 ) ) ;
#3440 = CARTESIAN_POINT ( 'NONE',  ( -16.68014207497104451, -3.425858445063780788, -215.9332308579483595 ) ) ;
#3441 = CARTESIAN_POINT ( 'NONE',  ( 13.55929460187270053, 0.3562519042583365270, -227.9787723277739246 ) ) ;
#3442 = CARTESIAN_POINT ( 'NONE',  ( 28.51464931495100785, 5.422321182929326966, -223.8116416110474347 ) ) ;
#3443 = CARTESIAN_POINT ( 'NONE',  ( -16.15126510923403202, -0.4755054218165427615, -219.3066569788202571 ) ) ;
#3444 = CARTESIAN_POINT ( 'NONE',  ( 24.80560757033128993, -15.22139526172250079, -221.3338856610240271 ) ) ;
#3445 = CARTESIAN_POINT ( 'NONE',  ( -16.65698539163286540, 11.03290537638306112, -233.6474915129378758 ) ) ;
#3446 = CARTESIAN_POINT ( 'NONE',  ( -13.98136146596813845, 3.850743984385103680, -228.7620665878280590 ) ) ;
#3447 = ADVANCED_FACE ( 'NONE', ( #8186 ), #19357, .T. ) ;
#3448 = CARTESIAN_POINT ( 'NONE',  ( 0.7797512750231831991, -26.58197935702783354, -230.4407411870234625 ) ) ;
#3449 = CARTESIAN_POINT ( 'NONE',  ( 0.000000000000000000, 0.000000000000000000, -120.0000000000000142 ) ) ;
#3450 = CARTESIAN_POINT ( 'NONE',  ( -22.94283062359114922, 1.652932088558951573, 9.867976570195974517 ) ) ;
#3451 = CARTESIAN_POINT ( 'NONE',  ( 0.000000000000000000, 0.000000000000000000, 60.00000000000001421 ) ) ;
#3452 = CARTESIAN_POINT ( 'NONE',  ( 13.39501375133567329, -10.34300172232987691, -228.1452887455185987 ) ) ;
#3453 = AXIS2_PLACEMENT_3D ( 'NONE', #585, #10608, #7460 ) ;
#3454 = CARTESIAN_POINT ( 'NONE',  ( 12.82662589338795556, -3.005951546645926786, -225.0248285060761759 ) ) ;
#3455 = CARTESIAN_POINT ( 'NONE',  ( -21.30687190786788676, -8.669990142398665611, -5.025571895822516844 ) ) ;
#3456 = CARTESIAN_POINT ( 'NONE',  ( 9.653903571287008489, 19.16609876806546353, -219.1149796918802792 ) ) ;
#3457 = CARTESIAN_POINT ( 'NONE',  ( 5.909674498212842408, 15.76475534640655773, -228.4922217450045139 ) ) ;
#3458 = CARTESIAN_POINT ( 'NONE',  ( 20.52151979663716830, -23.02670487196117222, -229.5295066797569348 ) ) ;
#3459 = CARTESIAN_POINT ( 'NONE',  ( 11.31395536621571019, -8.070181239749643964, -225.0898076798974614 ) ) ;
#3460 = ORIENTED_EDGE ( 'NONE', *, *, #8010, .F. ) ;
#3461 = PRODUCT_DEFINITION_FORMATION_WITH_SPECIFIED_SOURCE ( 'ANY', '', #6909, .NOT_KNOWN. ) ;
#3462 = CARTESIAN_POINT ( 'NONE',  ( -11.08731210905863840, 25.61052584666692766, -228.9953606804266997 ) ) ;
#3463 = CARTESIAN_POINT ( 'NONE',  ( -15.47996233766743934, 8.203483081506188768, -221.0931279926996353 ) ) ;
#3464 = CARTESIAN_POINT ( 'NONE',  ( -14.37318171526297483, 2.227741863946853140, -231.7654527934561202 ) ) ;
#3465 = ORIENTED_EDGE ( 'NONE', *, *, #250, .F. ) ;
#3466 = CARTESIAN_POINT ( 'NONE',  ( -1.044869047506413517, -25.54243019362050404, -231.6194713969048564 ) ) ;
#3467 = CARTESIAN_POINT ( 'NONE',  ( 25.50000000000000000, -0.5000000000000000000, -6.000000000000000000 ) ) ;
#3468 = VERTEX_POINT ( 'NONE', #8412 ) ;
#3469 = CARTESIAN_POINT ( 'NONE',  ( 24.78377098693636427, 3.871650763546384155, -231.3521132786341923 ) ) ;
#3470 = CARTESIAN_POINT ( 'NONE',  ( 13.61677703237491777, -11.64725695657166682, -220.6715806775949034 ) ) ;
#3471 = CARTESIAN_POINT ( 'NONE',  ( 8.812073984913094904, 13.12649198322903210, -229.9172071780580495 ) ) ;
#3472 = CARTESIAN_POINT ( 'NONE',  ( -24.02434186778878455, 18.57431834865475651, -228.2662945587547370 ) ) ;
#3473 = CARTESIAN_POINT ( 'NONE',  ( 14.81251837262747983, -1.020578734748967209, -221.0290343291311785 ) ) ;
#3474 = ADVANCED_FACE ( 'NONE', ( #12002 ), #15162, .T. ) ;
#3475 = CARTESIAN_POINT ( 'NONE',  ( 6.093530912645064745, 16.79941505724243811, -232.1766444656230419 ) ) ;
#3476 = CARTESIAN_POINT ( 'NONE',  ( 27.04607490430786854, 4.607450003618843049, -220.3758934308003461 ) ) ;
#3477 = CARTESIAN_POINT ( 'NONE',  ( 1.752757082432757185, -17.15725705531007250, -232.7539178101738742 ) ) ;
#3478 = CARTESIAN_POINT ( 'NONE',  ( 23.44296991241933981, -12.51566675729016964, -231.4065378011870564 ) ) ;
#3479 = CARTESIAN_POINT ( 'NONE',  ( 0.000000000000000000, 19.79999999999999716, -78.50000000000000000 ) ) ;
#3480 = PRODUCT_DEFINITION_SHAPE ( 'NONE', 'NONE',  #6018 ) ;
#3481 = CARTESIAN_POINT ( 'NONE',  ( 2.985191413800211088E-29, 21.63401512838760610, -77.51594804401857175 ) ) ;
#3482 = CARTESIAN_POINT ( 'NONE',  ( -20.87212828950092813, -0.8819659211619411687, -215.0000000018925448 ) ) ;
#3483 = CARTESIAN_POINT ( 'NONE',  ( -12.33332453308451804, -15.34461866416700282, -218.5928953102074388 ) ) ;
#3484 = CARTESIAN_POINT ( 'NONE',  ( 7.680972971696337304, -18.49313070787806623, -217.8811398819712508 ) ) ;
#3485 = EDGE_CURVE ( 'NONE', #5014, #19761, #15408, .T. ) ;
#3486 = CARTESIAN_POINT ( 'NONE',  ( -26.02492405343843984, 6.940268742526972900, -218.8798307745116460 ) ) ;
#3487 = CARTESIAN_POINT ( 'NONE',  ( 10.25948093768852054, 28.38842464930171872, -224.3436940787075855 ) ) ;
#3488 = CARTESIAN_POINT ( 'NONE',  ( -16.23478446547628096, 26.31175924651574149, -222.4178907105033431 ) ) ;
#3489 = ORIENTED_EDGE ( 'NONE', *, *, #10673, .F. ) ;
#3490 = CARTESIAN_POINT ( 'NONE',  ( 18.01918173885548313, -1.728726289433203611, -215.5890043894241330 ) ) ;
#3491 = ORIENTED_EDGE ( 'NONE', *, *, #7092, .F. ) ;
#3492 = CARTESIAN_POINT ( 'NONE',  ( 23.04897566969193079, 17.95862962700741861, -223.6438515760422661 ) ) ;
#3493 = CARTESIAN_POINT ( 'NONE',  ( -11.19223248830523332, 8.463078350427430507, -222.6400917074981578 ) ) ;
#3494 = CARTESIAN_POINT ( 'NONE',  ( -18.63458318964815774, 8.046101765467303935, -217.8151248213926863 ) ) ;
#3495 = CARTESIAN_POINT ( 'NONE',  ( -19.43452863239301820, -21.19996443032342626, -221.1427059245750399 ) ) ;
#3496 = DIRECTION ( 'NONE',  ( 0.000000000000000000, 0.000000000000000000, -1.000000000000000000 ) ) ;
#3497 = CARTESIAN_POINT ( 'NONE',  ( 13.86383614057800884, 4.939477956453596441, -219.6543243356308324 ) ) ;
#3498 = CARTESIAN_POINT ( 'NONE',  ( -18.02718827071834085, 20.33515877052379395, -229.5060669840136143 ) ) ;
#3499 = CARTESIAN_POINT ( 'NONE',  ( 22.66015888791822519, 10.43487984001084534, -234.3950629709119937 ) ) ;
#3500 = CARTESIAN_POINT ( 'NONE',  ( 17.81160404892403193, 9.939217752910943560, -216.9646549374535311 ) ) ;
#3501 = CARTESIAN_POINT ( 'NONE',  ( -30.53557093151922430, -9.496448454471346778, -222.0905184547210638 ) ) ;
#3502 = VERTEX_POINT ( 'NONE', #9985 ) ;
#3503 = CARTESIAN_POINT ( 'NONE',  ( -8.011291865669539547, -12.94570094964118923, -221.6322823144945744 ) ) ;
#3504 = CARTESIAN_POINT ( 'NONE',  ( -6.331039912586185814, 17.62337457105953220, -233.2305561356360499 ) ) ;
#3505 = CARTESIAN_POINT ( 'NONE',  ( 6.260999666360449467, -13.19315344885661645, -220.2890618333529744 ) ) ;
#3506 = CARTESIAN_POINT ( 'NONE',  ( -3.643097910890548796, 22.16888955197135047, -233.9701981029593298 ) ) ;
#3507 = CARTESIAN_POINT ( 'NONE',  ( 16.95735638057670869, -14.83641200555466355, -235.2222363121530293 ) ) ;
#3508 = CARTESIAN_POINT ( 'NONE',  ( -16.21268175593173311, -5.852138355245464219, -231.1837890105803410 ) ) ;
#3509 = CARTESIAN_POINT ( 'NONE',  ( 29.01678366425524658, 8.126504218505314014, -229.6975090854573125 ) ) ;
#3510 = CARTESIAN_POINT ( 'NONE',  ( 0.000000000000000000, 0.000000000000000000, -120.0000000000000142 ) ) ;
#3511 = CARTESIAN_POINT ( 'NONE',  ( -6.208492967940078877, 16.71913201805454463, -230.4912298573936766 ) ) ;
#3512 = CARTESIAN_POINT ( 'NONE',  ( -18.05576253097465766, 2.935622250037499104, -232.1557308718028594 ) ) ;
#3513 = CARTESIAN_POINT ( 'NONE',  ( 7.995304978256253747, 13.28024228361502779, -220.6535174700288451 ) ) ;
#3514 = CARTESIAN_POINT ( 'NONE',  ( 26.06405806384012536, 5.488112530166501024, -216.5020692413490622 ) ) ;
#3515 = CARTESIAN_POINT ( 'NONE',  ( 4.525470981882147470, -27.64997114140619416, -217.1529231092339103 ) ) ;
#3516 = CARTESIAN_POINT ( 'NONE',  ( 2.471991688031208945, 13.88348721647344419, -230.6707754746932437 ) ) ;
#3517 = CARTESIAN_POINT ( 'NONE',  ( 0.000000000000000000, 0.000000000000000000, -77.51594804401857175 ) ) ;
#3518 = CARTESIAN_POINT ( 'NONE',  ( -8.215923615656011592, -19.99105411527736820, -235.1422105638354481 ) ) ;
#3519 = CARTESIAN_POINT ( 'NONE',  ( -16.84845737324940984, 22.31296517946017488, -228.8910390263689010 ) ) ;
#3520 = CARTESIAN_POINT ( 'NONE',  ( 2.535512286608554433, 13.86868953312499109, -224.9313928733152181 ) ) ;
#3521 = CARTESIAN_POINT ( 'NONE',  ( -15.19144047750087267, -10.24270553329939304, -232.4311702607364793 ) ) ;
#3522 = CARTESIAN_POINT ( 'NONE',  ( -21.18474081038989354, 8.486062504918864491, -230.7949373529753530 ) ) ;
#3523 = AXIS2_PLACEMENT_3D ( 'NONE', #14795, #4540, #21526 ) ;
#3524 = CARTESIAN_POINT ( 'NONE',  ( 13.09827881591457022, 28.40264942367575784, -221.1045935444571455 ) ) ;
#3525 = ORIENTED_EDGE ( 'NONE', *, *, #13692, .T. ) ;
#3526 = CARTESIAN_POINT ( 'NONE',  ( 4.730976410881341465, 17.65764351829336931, -217.6025626048331674 ) ) ;
#3527 = CARTESIAN_POINT ( 'NONE',  ( 14.02135871364020936, -4.809710560857269002, -224.5109434094503911 ) ) ;
#3528 = CARTESIAN_POINT ( 'NONE',  ( 16.18295504345472580, -4.390854861972272261, -232.0514848646187716 ) ) ;
#3529 = CARTESIAN_POINT ( 'NONE',  ( -3.010752168931037698, 15.84372070116375575, -223.4060793985500482 ) ) ;
#3530 = SURFACE_STYLE_USAGE ( .BOTH. , #18954 ) ;
#3531 = CARTESIAN_POINT ( 'NONE',  ( 15.89706143421296147, 10.57416387607782227, -218.3862415393350318 ) ) ;
#3532 = CARTESIAN_POINT ( 'NONE',  ( -14.71809293534535534, -5.923356948231951691, -217.5005292165803041 ) ) ;
#3533 = CARTESIAN_POINT ( 'NONE',  ( -0.1947256686167265494, -30.94043057420685727, -223.1178397439027492 ) ) ;
#3534 = CARTESIAN_POINT ( 'NONE',  ( 21.39922646226391478, -21.53954253117021977, -224.1701659532164967 ) ) ;
#3535 = CARTESIAN_POINT ( 'NONE',  ( -6.564517230509238743, 23.65597541655194647, -219.1225629381441991 ) ) ;
#3536 = DIRECTION ( 'NONE',  ( 0.000000000000000000, 0.000000000000000000, 1.000000000000000000 ) ) ;
#3537 = CARTESIAN_POINT ( 'NONE',  ( 24.14003655968566520, 13.76285650325712773, -228.1266575292093819 ) ) ;
#3538 = ADVANCED_FACE ( 'NONE', ( #22237 ), #13622, .T. ) ;
#3539 = CARTESIAN_POINT ( 'NONE',  ( -24.02434186778878455, 18.57431834865475651, -228.2662945587547370 ) ) ;
#3540 = CARTESIAN_POINT ( 'NONE',  ( -15.72555926117677139, 17.60926865496976745, -217.2114552733360142 ) ) ;
#3541 = CARTESIAN_POINT ( 'NONE',  ( 15.91397826126795323, -3.183288324723350549, -218.2846031002558504 ) ) ;
#3542 = ORIENTED_EDGE ( 'NONE', *, *, #3964, .T. ) ;
#3543 = CARTESIAN_POINT ( 'NONE',  ( 5.955271202636533090, 21.50135983300913267, -233.0184468368920534 ) ) ;
#3544 = CARTESIAN_POINT ( 'NONE',  ( 21.04928763009552384, -0.2309942901367783852, -233.9427286327411366 ) ) ;
#3545 = CARTESIAN_POINT ( 'NONE',  ( 9.986779374595107228, 29.47523823012521049, -229.5287702428778687 ) ) ;
#3546 = CIRCLE ( 'NONE', #16861, 23.00000000000000000 ) ;
#3547 = CARTESIAN_POINT ( 'NONE',  ( 8.158223302632384488, -13.44420475212243993, -229.3230086144918403 ) ) ;
#3548 = CARTESIAN_POINT ( 'NONE',  ( -25.00000000000000000, 0.000000000000000000, 75.00000000000000000 ) ) ;
#3549 = ORIENTED_EDGE ( 'NONE', *, *, #3744, .T. ) ;
#3550 = CARTESIAN_POINT ( 'NONE',  ( -9.740348021262962064, 16.12529029871877384, -216.4361617420699702 ) ) ;
#3551 = CARTESIAN_POINT ( 'NONE',  ( -25.64743926792790063, -18.08564893845128907, -228.9187414798782925 ) ) ;
#3552 = CYLINDRICAL_SURFACE ( 'NONE', #11579, 23.00000000000008882 ) ;
#3553 = CARTESIAN_POINT ( 'NONE',  ( 21.53262694368047647, 11.06794636811408594, -231.8394491640143826 ) ) ;
#3554 = CARTESIAN_POINT ( 'NONE',  ( -21.08008464085897060, -0.9048411197481797119, -217.0000000010748522 ) ) ;
#3555 = CARTESIAN_POINT ( 'NONE',  ( 14.68556740487494849, -6.365102927765655672, -229.6664356779805587 ) ) ;
#3556 =( LENGTH_UNIT ( ) NAMED_UNIT ( * ) SI_UNIT ( .MILLI., .METRE. ) );
#3557 = CARTESIAN_POINT ( 'NONE',  ( -8.966714183099560032, 19.05224306381768073, -234.0879867025980445 ) ) ;
#3558 = CARTESIAN_POINT ( 'NONE',  ( -20.54164754914381064, 7.122791156791981493, -233.5720402887671980 ) ) ;
#3559 = CARTESIAN_POINT ( 'NONE',  ( -0.3025942668150596315, -28.96010673020088788, -223.5534481764385646 ) ) ;
#3560 = DIRECTION ( 'NONE',  ( -0.000000000000000000, 0.000000000000000000, -1.000000000000000000 ) ) ;
#3561 = CARTESIAN_POINT ( 'NONE',  ( -20.95737978171097993, 9.479626318133300700, 3.249830451118298047 ) ) ;
#3562 = CARTESIAN_POINT ( 'NONE',  ( -12.31207293045244988, 6.732038552366256923, -221.0952066824360713 ) ) ;
#3563 = CARTESIAN_POINT ( 'NONE',  ( 13.96153919378708075, -19.04487818418218481, -231.5728976975466367 ) ) ;
#3564 = CARTESIAN_POINT ( 'NONE',  ( 13.66359280701490420, -1.647215465832199355, -222.4923211118234008 ) ) ;
#3565 = EDGE_CURVE ( 'NONE', #8742, #7031, #18647, .T. ) ;
#3566 = CARTESIAN_POINT ( 'NONE',  ( -24.99351254083359208, 0.6581337445957534671, 9.983815384650208458 ) ) ;
#3567 = CARTESIAN_POINT ( 'NONE',  ( 13.72034832542693827, 10.98995328009155692, -220.6189139471235592 ) ) ;
#3568 = CARTESIAN_POINT ( 'NONE',  ( -7.329856113536736828, 10.17606210583481818, -226.3085553030691415 ) ) ;
#3569 = CARTESIAN_POINT ( 'NONE',  ( 19.59567110982616001, 18.11097967140601028, -228.7314497914969706 ) ) ;
#3570 = CARTESIAN_POINT ( 'NONE',  ( -5.427686778165598191, -19.74436295060356272, -231.6150980610854901 ) ) ;
#3571 = CARTESIAN_POINT ( 'NONE',  ( 11.88751558872989378, -3.770303194171726435, -225.3699946362665969 ) ) ;
#3572 = VERTEX_POINT ( 'NONE', #6600 ) ;
#3573 = CARTESIAN_POINT ( 'NONE',  ( -2.435715273212520238, 23.41098772907853132, -217.6796576669356966 ) ) ;
#3574 = CARTESIAN_POINT ( 'NONE',  ( -18.92390258637512090, 12.75887082072172163, -230.9970325548277970 ) ) ;
#3575 = CARTESIAN_POINT ( 'NONE',  ( -20.05025075566126702, 1.207204931470905018, -215.1628017022767949 ) ) ;
#3576 = CARTESIAN_POINT ( 'NONE',  ( -8.785593564164850378, -26.69987990810942691, -222.9015467003982849 ) ) ;
#3577 = CARTESIAN_POINT ( 'NONE',  ( 23.06814834742187514, -2.825033403592650701E-15, -74.48236190979496030 ) ) ;
#3578 = ORIENTED_EDGE ( 'NONE', *, *, #16995, .T. ) ;
#3579 = CARTESIAN_POINT ( 'NONE',  ( 27.79670308438203108, 10.67628923451848877, -225.2981230784098727 ) ) ;
#3580 = CARTESIAN_POINT ( 'NONE',  ( 21.81705645104102587, -16.14081802208856686, -221.4047148572338131 ) ) ;
#3581 = CARTESIAN_POINT ( 'NONE',  ( 4.559463107227270662, 13.27337529356814017, -226.9596205199204633 ) ) ;
#3582 = CARTESIAN_POINT ( 'NONE',  ( -13.55591840520136770, 8.363404288414606924, -231.2690188357804857 ) ) ;
#3583 = CARTESIAN_POINT ( 'NONE',  ( 30.57915561709945251, 3.468229287067555067, -223.8876084027091906 ) ) ;
#3584 = CARTESIAN_POINT ( 'NONE',  ( 8.979547488457603421, 23.24376652602565230, -232.6628827740196357 ) ) ;
#3585 = CARTESIAN_POINT ( 'NONE',  ( 13.77325227673554942, 1.931642680738434148, -222.7035726732354703 ) ) ;
#3586 = CARTESIAN_POINT ( 'NONE',  ( -0.6367083786117293531, -29.73461014436635708, -220.1383336929387724 ) ) ;
#3587 = CARTESIAN_POINT ( 'NONE',  ( 15.54083024098960486, -10.44392130763852222, -217.6620978190037476 ) ) ;
#3588 = CARTESIAN_POINT ( 'NONE',  ( 0.000000000000000000, 0.000000000000000000, 75.00000000000000000 ) ) ;
#3589 = DIRECTION ( 'NONE',  ( -0.000000000000000000, -0.000000000000000000, 1.000000000000000000 ) ) ;
#3590 = CARTESIAN_POINT ( 'NONE',  ( -11.87391433320165746, 8.920676825367966245, -232.2044275666449096 ) ) ;
#3591 = CARTESIAN_POINT ( 'NONE',  ( -18.09422283036245460, -3.216155923901089064, -229.6485988878351918 ) ) ;
#3592 = CARTESIAN_POINT ( 'NONE',  ( 13.71882454279727526, 6.278400000045776252, -230.2269611870541723 ) ) ;
#3593 = CARTESIAN_POINT ( 'NONE',  ( 8.674175678922351196, 20.85307874897338110, -216.6688793998777101 ) ) ;
#3594 = CARTESIAN_POINT ( 'NONE',  ( 3.522445101072706475, 23.08420003150784439, -231.7850044194335055 ) ) ;
#3595 = ORIENTED_EDGE ( 'NONE', *, *, #16262, .F. ) ;
#3596 = CARTESIAN_POINT ( 'NONE',  ( -24.19871179313096476, -3.348666575842360160, -230.4488973568908534 ) ) ;
#3597 = CARTESIAN_POINT ( 'NONE',  ( 11.62313423782632782, 11.98467543564608029, -219.7293303032897995 ) ) ;
#3598 = EDGE_CURVE ( 'NONE', #758, #12912, #16124, .T. ) ;
#3599 = CARTESIAN_POINT ( 'NONE',  ( -24.33894786102607455, 16.69464852328507831, -227.6320542475859554 ) ) ;
#3600 = CARTESIAN_POINT ( 'NONE',  ( -17.89085717681497201, 10.08962028281416856, -232.3705156551908431 ) ) ;
#3601 = CARTESIAN_POINT ( 'NONE',  ( -22.54883021006152433, -16.50439104605484530, -230.5104955902558004 ) ) ;
#3602 = CARTESIAN_POINT ( 'NONE',  ( -14.10849459794400751, -0.2436790717799666162, -223.1085195285415921 ) ) ;
#3603 = DIRECTION ( 'NONE',  ( 0.1093404791528972547, -0.9940043559354329039, 0.000000000000000000 ) ) ;
#3604 = CARTESIAN_POINT ( 'NONE',  ( 15.39025625686376841, 1.044190007782545226, -218.9203249718910911 ) ) ;
#3605 = CARTESIAN_POINT ( 'NONE',  ( -17.07311071032027172, 18.59516984069744794, -230.9440421721702137 ) ) ;
#3606 = CARTESIAN_POINT ( 'NONE',  ( 5.179557175392591972, 10.46258103618983881, -224.6216839350439614 ) ) ;
#3607 = CARTESIAN_POINT ( 'NONE',  ( -14.29986196492902550, 0.06805469746732484282, -227.4167624117703213 ) ) ;
#3608 = CARTESIAN_POINT ( 'NONE',  ( -14.38198375515248273, -6.747285987484331393, -233.1569015480179985 ) ) ;
#3609 = EDGE_LOOP ( 'NONE', ( #11113, #11248, #19713, #2392 ) ) ;
#3610 = CARTESIAN_POINT ( 'NONE',  ( -14.01584329375060456, -3.774282517739922405, -220.6818330080343173 ) ) ;
#3611 = CARTESIAN_POINT ( 'NONE',  ( -4.591517861330576267, 12.55780501983563191, -223.5932882008353033 ) ) ;
#3612 = CARTESIAN_POINT ( 'NONE',  ( -8.803769170443210612, -17.82266517633203406, -233.6972128408098683 ) ) ;
#3613 = CARTESIAN_POINT ( 'NONE',  ( -5.807479211365208727, 19.77444019604324410, -216.0778658752277863 ) ) ;
#3614 = CARTESIAN_POINT ( 'NONE',  ( 30.13983206778957324, -7.413543662652124944, -226.8644184361555745 ) ) ;
#3615 = FACE_OUTER_BOUND ( 'NONE', #253, .T. ) ;
#3616 = CARTESIAN_POINT ( 'NONE',  ( 15.14536540539411114, 2.907144070186200580, -217.8738854795238922 ) ) ;
#3617 = CARTESIAN_POINT ( 'NONE',  ( 0.000000000000000000, 0.000000000000000000, -77.51594804401857175 ) ) ;
#3618 = CARTESIAN_POINT ( 'NONE',  ( 0.1979841192334154676, 16.22068729745496540, -223.9539336445596973 ) ) ;
#3619 = CARTESIAN_POINT ( 'NONE',  ( -14.07336028695978314, 1.752429266630609828, -222.9750305084206161 ) ) ;
#3620 = CARTESIAN_POINT ( 'NONE',  ( 18.54610009393809023, 0.6523581019769808531, -231.1787333216317677 ) ) ;
#3621 = CARTESIAN_POINT ( 'NONE',  ( 25.85827166240959940, 13.84420748389600675, -220.2831452073696425 ) ) ;
#3622 = CARTESIAN_POINT ( 'NONE',  ( -3.771778814064143504, -12.72945944931849915, -225.7745976896340778 ) ) ;
#3623 = CARTESIAN_POINT ( 'NONE',  ( 1.833772325875588027, 13.50593961039006707, -219.8748197804281119 ) ) ;
#3624 = CARTESIAN_POINT ( 'NONE',  ( 22.03647168420945590, 0.3315607655625663064, -232.0572713672586644 ) ) ;
#3625 = CARTESIAN_POINT ( 'NONE',  ( -3.564252528062037406, -12.01378896085460291, -227.6748268428467270 ) ) ;
#3626 = CARTESIAN_POINT ( 'NONE',  ( -11.48592899399814726, 13.65854631785387774, -230.8311022452805616 ) ) ;
#3627 = CARTESIAN_POINT ( 'NONE',  ( 15.37089934297015503, 20.64239674606488961, -217.2018742121147170 ) ) ;
#3628 = CARTESIAN_POINT ( 'NONE',  ( -28.55814054826834791, -1.660722980825670048, -228.2640858091212408 ) ) ;
#3629 = CARTESIAN_POINT ( 'NONE',  ( -16.58624905143161143, 8.715293938925766426, -220.0618460037763384 ) ) ;
#3630 = EDGE_CURVE ( 'NONE', #4483, #16572, #12535, .T. ) ;
#3631 = CARTESIAN_POINT ( 'NONE',  ( -5.373457274256926652, 30.83572167890261184, -229.2199105909169532 ) ) ;
#3632 = CARTESIAN_POINT ( 'NONE',  ( 17.89221702206198117, 0.2742047965568425449, -220.2420650470893122 ) ) ;
#3633 = ORIENTED_EDGE ( 'NONE', *, *, #20686, .F. ) ;
#3634 = CARTESIAN_POINT ( 'NONE',  ( 18.79065350309113214, -20.33706828427738600, -226.6662063318914591 ) ) ;
#3635 = CARTESIAN_POINT ( 'NONE',  ( 4.725966861008204845, -14.24791254766627624, -227.2781441550517343 ) ) ;
#3636 = CARTESIAN_POINT ( 'NONE',  ( -5.125319492185865577, 20.53749879880200524, -218.7557759432853288 ) ) ;
#3637 = CARTESIAN_POINT ( 'NONE',  ( 14.39473142419577023, 15.98257177912839389, -217.4557725731239373 ) ) ;
#3638 = CARTESIAN_POINT ( 'NONE',  ( -14.73876579896802141, -0.4225899574144328374, -230.2531052195884342 ) ) ;
#3639 = CARTESIAN_POINT ( 'NONE',  ( -1.542335193334551491, -19.71915426430242135, -216.1352730594569209 ) ) ;
#3640 = CARTESIAN_POINT ( 'NONE',  ( 6.166782020495575445, -26.61202787628535660, -217.6604608484729795 ) ) ;
#3641 = CARTESIAN_POINT ( 'NONE',  ( -8.316066124693966444, 26.67103469786491843, -222.2304303634109885 ) ) ;
#3642 = FACE_OUTER_BOUND ( 'NONE', #11362, .T. ) ;
#3643 = CARTESIAN_POINT ( 'NONE',  ( 21.07144422417032104, 18.33581350331571969, -223.6711752364813890 ) ) ;
#3644 = CARTESIAN_POINT ( 'NONE',  ( -23.52999999174766543, 19.39566142560855866, -221.9446938626390704 ) ) ;
#3645 = CARTESIAN_POINT ( 'NONE',  ( -5.764806379010653181, 14.19340719117484007, -223.8851086052821415 ) ) ;
#3646 = CARTESIAN_POINT ( 'NONE',  ( -0.5888410438786807477, 14.99789765555501475, -227.7044550383138244 ) ) ;
#3647 = CARTESIAN_POINT ( 'NONE',  ( 13.93840998928060415, 0.7705246578886114639, -220.8158265847476116 ) ) ;
#3648 = CARTESIAN_POINT ( 'NONE',  ( 19.48863273024974418, 12.80680990455712909, -215.0408095016468053 ) ) ;
#3649 = CARTESIAN_POINT ( 'NONE',  ( 9.835929410207317147, -16.71508016877321268, -232.2716196330763694 ) ) ;
#3650 = FACE_OUTER_BOUND ( 'NONE', #20250, .T. ) ;
#3651 = VERTEX_POINT ( 'NONE', #15280 ) ;
#3652 = CARTESIAN_POINT ( 'NONE',  ( -0.9414827276148034496, 23.96885519606619752, -216.4491898092606164 ) ) ;
#3653 = CARTESIAN_POINT ( 'NONE',  ( 16.03897629125586377, -3.546747291816754633, -223.1229430630804700 ) ) ;
#3654 = CARTESIAN_POINT ( 'NONE',  ( 20.15756451863428111, -2.090604891399794774, -217.8900786001194945 ) ) ;
#3655 = CIRCLE ( 'NONE', #16244, 1.000000000000000888 ) ;
#3656 = CARTESIAN_POINT ( 'NONE',  ( 23.04897566969193079, 17.95862962700741861, -223.6438515760422661 ) ) ;
#3657 = CARTESIAN_POINT ( 'NONE',  ( -17.88126539071149779, 5.766250685202066961, -232.9050303536861293 ) ) ;
#3658 = CARTESIAN_POINT ( 'NONE',  ( 8.510712203779903007, -27.79691582975998898, -230.5316902582456180 ) ) ;
#3659 = CARTESIAN_POINT ( 'NONE',  ( -9.540790481621398200, 9.981116473660406996, -228.6478862620407995 ) ) ;
#3660 = ORIENTED_EDGE ( 'NONE', *, *, #1264, .F. ) ;
#3661 = CARTESIAN_POINT ( 'NONE',  ( -23.49379658590067876, 11.46840048879614393, -217.2519070826072323 ) ) ;
#3662 = CARTESIAN_POINT ( 'NONE',  ( -10.94940667656068634, -10.80050631132953498, -220.7362776234490127 ) ) ;
#3663 = DIRECTION ( 'NONE',  ( 0.000000000000000000, 0.000000000000000000, -1.000000000000000000 ) ) ;
#3664 = CARTESIAN_POINT ( 'NONE',  ( -22.44443514569313081, 5.033247747886526291, 8.647138457592827621 ) ) ;
#3665 = CARTESIAN_POINT ( 'NONE',  ( -24.02434186778878455, 18.57431834865475651, -228.2662945587547370 ) ) ;
#3666 = CARTESIAN_POINT ( 'NONE',  ( 13.82101996411362244, -10.82539765916244789, -229.0162845096555770 ) ) ;
#3667 = DIRECTION ( 'NONE',  ( 0.000000000000000000, -1.000000000000000000, 0.000000000000000000 ) ) ;
#3668 = CIRCLE ( 'NONE', #19490, 20.99999999999999645 ) ;
#3669 = CARTESIAN_POINT ( 'NONE',  ( 19.25067847059915849, -2.577822808762990636, -226.5499581033751895 ) ) ;
#3670 = CARTESIAN_POINT ( 'NONE',  ( 26.92457506054779515, 6.538608665672222209, -219.8654465082432807 ) ) ;
#3671 = CARTESIAN_POINT ( 'NONE',  ( -16.23478446547628096, 26.31175924651574149, -222.4178907105033431 ) ) ;
#3672 = LINE ( 'NONE', #320, #8873 ) ;
#3673 = CARTESIAN_POINT ( 'NONE',  ( 12.91676121433235913, 9.519065828383201477, -226.8102878246443765 ) ) ;
#3674 = CARTESIAN_POINT ( 'NONE',  ( -3.373690338999510985, -20.30281967708846125, -218.2431319494177160 ) ) ;
#3675 = CARTESIAN_POINT ( 'NONE',  ( -23.14980455159086503, 0.3541108476526578785, -217.8785187302087536 ) ) ;
#3676 = ORIENTED_EDGE ( 'NONE', *, *, #8689, .T. ) ;
#3677 = CARTESIAN_POINT ( 'NONE',  ( -4.583529401292260275, 28.77615850237956607, -226.7744741901706504 ) ) ;
#3678 = CARTESIAN_POINT ( 'NONE',  ( -22.38528940623734798, 16.50235888036280230, -227.1443357386333162 ) ) ;
#3679 = CARTESIAN_POINT ( 'NONE',  ( 14.32363442937021425, 2.978337679677412808, -227.0386046113487453 ) ) ;
#3680 = CARTESIAN_POINT ( 'NONE',  ( -21.81769295881711557, -14.18202798484824534, -220.2668003432649471 ) ) ;
#3681 = DIRECTION ( 'NONE',  ( -0.000000000000000000, -0.000000000000000000, 1.000000000000000000 ) ) ;
#3682 = VERTEX_POINT ( 'NONE', #4904 ) ;
#3683 = CARTESIAN_POINT ( 'NONE',  ( 28.56567312134318826, 3.451746495494312672, -224.1550573921799412 ) ) ;
#3684 = CARTESIAN_POINT ( 'NONE',  ( 0.5565384680698680642, -16.73444667301361122, -219.8404036742738015 ) ) ;
#3685 = CARTESIAN_POINT ( 'NONE',  ( 11.87982377808925527, 10.85265283465803421, -229.5027252913499183 ) ) ;
#3686 = CARTESIAN_POINT ( 'NONE',  ( -9.517741096562200909, 20.63709896626785678, -234.1036702156204967 ) ) ;
#3687 = TOROIDAL_SURFACE ( 'NONE', #6567, 24.63401512838748530, 3.000000000000004441 ) ;
#3688 = AXIS2_PLACEMENT_3D ( 'NONE', #12548, #7157, #12442 ) ;
#3689 = CARTESIAN_POINT ( 'NONE',  ( 18.03440114592047649, 4.755211820135348155, -216.3599228381250157 ) ) ;
#3690 = CARTESIAN_POINT ( 'NONE',  ( 12.10245006109274080, 26.02147364279441888, -220.6079829738538649 ) ) ;
#3691 = DIRECTION ( 'NONE',  ( 0.000000000000000000, 0.000000000000000000, -1.000000000000000000 ) ) ;
#3692 = CARTESIAN_POINT ( 'NONE',  ( 2.178520447619924472, -13.56847537563065487, -221.4085897031499428 ) ) ;
#3693 = CARTESIAN_POINT ( 'NONE',  ( 8.818493748348606331, -10.89961555176610375, -227.9481955143288303 ) ) ;
#3694 = DIRECTION ( 'NONE',  ( 1.000000000000000000, 0.000000000000000000, 0.000000000000000000 ) ) ;
#3695 = CARTESIAN_POINT ( 'NONE',  ( -22.63401512838748175, 0.000000000000000000, -77.51594804401857175 ) ) ;
#3696 = CARTESIAN_POINT ( 'NONE',  ( -8.653738780971721667, 11.12943719949617893, -219.7525355316396087 ) ) ;
#3697 = CARTESIAN_POINT ( 'NONE',  ( -16.45250455720563210, -7.911775896682759601, -220.5271995834187067 ) ) ;
#3698 = VECTOR ( 'NONE', #18705, 1000.000000000000000 ) ;
#3699 =( BOUNDED_SURFACE ( )  B_SPLINE_SURFACE ( 3, 3, ( 
 ( #5962, #12839, #19683, #4600, #20119, #16993, #9682, #6295, #15316, #20458, #6752, #6406, #1575, #10017, #21927, #14861, #13620, #11923, #8110, #8447, #5046, #6635, #13169, #3136, #11702, #14976, #9790, #15200, #1120, #18789, #22163, #16541, #16881, #11477, #11584, #13276, #7996, #21704, #1456, #20014, #4707, #15091, #6517, #11815, #18344, #2905, #16655, #4825, #3244, #1236, #21817, #13506, #18458, #20343, #22046, #4939, #18682, #3021, #9906, #16769, #1348, #13386, #8219, #18572, #20230, #8329, #10128, #3582, #10572, #6861, #106, #335, #10459, #17213, #8999, #3472, #439, #15862, #17553, #17441, #5609, #8559, #1897, #18898, #2010, #17320, #13958, #14184, #3805, #20685, #15423, #8892, #8781, #15642, #7313, #21021, #14632, #2120, #6977, #13729, #222, #15756, #10689, #12489, #7091, #3357, #5491, #10240, #20794, #13848, #5374, #14069, #7203, #20905, #20569, #5267, #17106, #1685, #5157, #12037, #10350, #1787, #12147, #8662, #3686, #12258, #15524, #19003, #19109, #12375, #19226, #986, #16297, #548, #12814, #21342, #17774, #19437, #2553, #10792, #21562, #18098, #7860, #19658, #21127, #21233, #655, #3916, #6152, #11123, #14726, #7533, #2447, #9330, #21455, #17659, #19336, #12592, #14507, #12919, #10898, #9549, #873, #2339, #7751, #9437, #14621, #6044, #14401, #5823, #12702, #16410, #762, #2226, #5936, #19549, #5715, #16190, #4138, #4243, #7425, #16086, #19765, #11017, #9223, #2666, #4022, #9107, #15974, #11229, #17991, #14294, #17885, #7638, #4345, #20199, #4680, #1318, #1539, #13474, #8083, #18212, #18541, #13248, #11555, #2773, #13143, #19987, #6486, #16740, #1427, #9654, #16515, #4574, #1092, #11450, #13027, #8191, #21898, #15058, #11670, #11788, #18427, #7966, #14832, #16851, #21675, #6268, #18318, #2878, #9760, #9875, #21789, #4794, #18654, #16625, #1206, #20314, #20093, #2991, #4909, #13355, #3107, #3215, #10098, #14951, #19874, #11342, #15167, #9990, #6376, #8301, #22009, #16962, #6605, #8417, #15286, #22134, #4461, #3656, #2090, #5126, #8636, #19080, #8968, #22242, #10209, #12007, #15833, #3771, #20764, #5346, #7061, #302, #1762, #18758, #13592, #10322, #15610, #13929, #6833, #3553, #17077, #18867, #1656, #10431, #3326, #5019, #19194, #20873, #7172, #12119, #17291, #20537, #15496, #18974, #12228, #17185, #8530, #11894, #6723, #74, #1867, #13701, #20655, #10539, #8747, #12341, #14037, #20430, #190, #5459, #17408, #15394, #3442, #6945, #13816, #5238, #10657, #1980, #8861, #15725, #17523, #10764, #7284, #409, #5578, #14153, #20990, #17629, #12458, #3884, #19306, #2196, #9077, #16988 ),
 ( #16649, #1231, #8105, #11811, #18678, #4935, #13501, #13382, #1568, #4486, #20113, #14855, #6512, #13271, #9900, #10123, #22041, #14971, #11365, #4821, #21812, #4702, #18234, #21699, #6290, #15086, #3016, #10012, #2794, #9677, #13164, #16536, #20009, #21585, #16764, #8214, #1342, #20225, #20339, #3239, #8442, #1115, #6173, #2900, #7990, #18452, #11698, #6631, #13051, #11578, #19898, #1452, #4595, #21922, #9783, #6400, #16876, #18567, #3132, #11471, #8325, #18339, #15195, #7409, #17425, #8764, #12133, #16071, #318, #17538, #13944, #20889, #3900, #2104, #12578, #14279, #2323, #10674, #21113, #8985, #1881, #13833, #7187, #20669, #5253, #5699, #7075, #17644, #10776, #12244, #12475, #3568, #18988, #20778, #19421, #4007, #19094, #10883, #10445, #424, #17305, #19321, #9208, #14053, #10555, #3671, #14169, #5476, #17759, #6962, #21004, #5360, #1995, #8876, #15625, #12359, #15740, #19209, #205, #3790, #2210, #15848, #7299, #5594, #9092, #15959, #532, #9419, #7846, #6252, #2432, #19644, #4229, #12798, #14712, #14605, #4559, #7952, #21547, #747, #11108, #17977, #14817, #7735, #14492, #21440, #17870, #12687, #4444, #4121, #5806, #11002, #9315, #2540, #19751, #16283, #6138, #13127, #16176, #857, #1078, #6030, #12904, #21662, #4331, #11215, #19972, #11435, #7623, #7517, #21219, #2758, #13012, #19534, #19858, #18083, #18304, #21327, #2652, #9533, #2863, #9747, #11326, #641, #5921, #16393, #18195, #14386, #972, #9639, #16501, #11992, #13684, #8403, #15270, #16948, #10195, #11655, #6362, #1192, #20184, #3201, #1524, #16726, #13459, #20080, #6473, #4667, #20299, #13234, #14934, #6818, #8517, #17063, #21995, #4894, #21884, #18852, #11774, #1640, #4780, #18414, #21774, #3427, #9975, #18638, #1303, #8284, #13578, #10083, #22227, #15380, #16610, #22120, #20521, #6707, #11540, #8069, #16836, #2977, #9861, #5110, #8178, #5003, #20414, #13342, #11880, #15043, #18526, #3092, #1412, #15153, #6590, #18743, #3310, #3757, #1748, #15820, #5671, #3643, #12215, #507, #14024, #7383, #5444, #10524, #12106, #7158, #17394, #17509, #13801, #7045, #7268, #1968, #1852, #15929, #10417, #14251, #21084, #2182, #2076, #12549, #15483, #8846, #3537, #8956, #15712, #20860, #19396, #10750, #5333, #56, #396, #289, #12326, #6930, #17278, #8730, #10642, #19181, #20977, #20640, #5225, #15597, #18961, #176, #10307, #14138, #5565, #12443, #19293, #9063, #17170, #8622, #13917, #20752, #19068, #3870, #17616, #2620, #11296, #16474, #17947, #14787, #6109, #4413, #14575, #7592, #4201, #14683, #9502, #11185, #21191, #18051, #21629, #11080 ),
 ( #941, #21411, #9612, #18168, #6221, #7705, #2732, #6001, #5776, #10853, #2511, #17727, #2294, #1051, #4092, #21517, #7818, #9285, #16364, #614, #9179, #10969, #7924, #13096, #16146, #3979, #7489, #19723, #16042, #12980, #14358, #19616, #14461, #718, #19827, #9389, #12657, #19503, #17839, #2404, #21294, #5890, #12768, #16251, #826, #12873, #4303, #9833, #4868, #11627, #1613, #4980, #11747, #20053, #1276, #16694, #11855, #4748, #11513, #18499, #14904, #9720, #1495, #1162, #2838, #8037, #21745, #8150, #16809, #6444, #18613, #3284, #6335, #15015, #20387, #3061, #9950, #18720, #1385, #8260, #10169, #17038, #4640, #4532, #18277, #22089, #3174, #16581, #10058, #21855, #8492, #18383, #13314, #20155, #15356, #22203, #16922, #6792, #2946, #15127, #8375, #19943, #13208, #21966, #6559, #11408, #13431, #15244, #6680, #20272, #13552, #8699, #3401, #20496, #17251, #261, #20833, #13772, #10496, #17148, #3511, #1725, #17362, #10283, #11966, #3845, #5535, #14110, #19042, #1938, #18936, #15902, #8818, #20947, #1823, #15460, #18828, #481, #7014, #15683, #20611, #5305, #10611, #7131, #19265, #12413, #9037, #13997, #10725, #5415, #8599, #5085, #13888, #33, #6902, #17590, #5196, #2050, #17482, #10391, #19151, #12080, #15566, #146, #2157, #13660, #20725, #12187, #3618, #12297, #3729, #8928, #15795, #373, #7241, #7571, #21272, #12524, #7463, #14331, #804, #11056, #18030, #3954, #10829, #21165, #19373, #5752, #7356, #2488, #16228, #9368, #5980, #6085, #11274, #2709, #17700, #21495, #10943, #2268, #4180, #12855, #14662, #19805, #5863, #18143, #9480, #7797, #17924, #17815, #14437, #2599, #19697, #14552, #9151, #21388, #9592, #12744, #2380, #12961, #16455, #4389, #4067, #14223, #7683, #19591, #16013, #21059, #5647, #12632, #590, #19478, #4284, #9264, #11163, #16340, #16121, #695, #916, #14765, #3259, #22063, #11830, #16787, #2818, #2922, #4618, #7904, #10143, #15105, #18696, #11493, #6421, #13292, #3150, #21606, #4953, #16558, #18474, #16896, #14879, #13520, #20247, #6313, #11718, #6534, #4842, #13404, #18361, #9809, #16672, #20361, #4723, #1028, #3037, #1252, #9698, #20133, #8127, #8236, #4506, #20031, #18588, #14993, #21720, #6652, #1137, #6198, #13075, #15218, #21942, #19919, #11387, #21832, #8015, #10034, #11603, #9923, #13187, #18255, #1362, #1471, #8347, #3592, #12159, #15654, #15768, #20918, #12386, #6766, #8902, #20584, #22177, #13860, #234, #2022, #7215, #8674, #5507, #19121, #17453, #5278, #5170, #17225, #5384, #7104, #1911, #11939, #8793, #19236, #1798, #12052, #346, #3816, #14080, #13747 ),
 ( #20700, #17012, #19015, #18803, #1589, #15538, #8465, #15331, #13635, #17121, #12268, #20808, #6, #13968, #20470, #5062, #1699, #3373, #10254, #6875, #8571, #15436, #10469, #18909, #3701, #3486, #10362, #121, #6988, #10583, #17332, #14939, #18309, #18202, #10803, #14305, #561, #2869, #17787, #2240, #9237, #5621, #451, #14822, #14196, #15874, #21033, #12499, #7437, #7543, #19449, #2763, #16615, #19346, #21138, #11440, #2352, #16097, #9751, #668, #21552, #1197, #8074, #17669, #17563, #9009, #13132, #16506, #7328, #1083, #5725, #21780, #9122, #12605, #4036, #6367, #13239, #7957, #20084, #15984, #10915, #6143, #10699, #2132, #3928, #14717, #13017, #19863, #4449, #11331, #9644, #21667, #6257, #19978, #4565, #15385, #8521, #9980, #10200, #1308, #9865, #4785, #3432, #18857, #16841, #8627, #8182, #20419, #18418, #17067, #62, #20303, #8290, #1417, #11885, #18643, #15487, #11998, #18747, #11660, #15158, #22001, #10312, #11779, #18530, #3206, #21889, #16730, #22232, #15048, #6478, #13347, #20190, #6595, #1530, #13464, #3317, #17176, #3098, #4900, #5116, #10088, #16953, #1752, #8408, #15275, #6936, #13806, #22125, #11546, #2982, #6823, #1645, #6713, #13689, #13583, #4671, #5008, #20527, #1971, #10858, #617, #17620, #16046, #19071, #293, #10755, #7493, #13920, #1857, #3646, #20646, #17734, #12446, #19297, #20981, #14256, #15716, #10421, #5229, #8849, #7274, #5569, #20755, #17513, #8736, #10530, #15602, #2081, #17282, #18965, #2299, #12553, #21089, #3761, #8959, #17397, #12110, #15823, #5675, #7161, #180, #3543, #7050, #14028, #400, #5336, #12332, #2186, #20864, #19400, #5449, #12219, #19185, #10646, #14144, #9067, #3874, #15936, #511, #7387, #3983, #9183, #832, #21521, #19947, #16152, #11085, #14791, #21416, #6006, #6227, #4308, #2627, #13101, #4536, #14466, #21195, #12662, #16478, #19831, #4097, #4419, #9394, #11412, #21300, #16256, #17952, #18281, #16586, #11301, #9724, #12773, #7711, #18172, #1167, #7598, #17845, #19621, #14362, #2842, #6113, #12984, #14687, #7928, #14580, #10975, #5783, #2516, #946, #2736, #5896, #11190, #2409, #4206, #9291, #18056, #723, #19510, #12878, #19728, #21633, #9508, #16369, #7822, #9616, #1055, #2951, #6340, #21750, #8044, #14910, #18388, #9839, #4645, #16700, #13213, #20058, #11518, #1400, #11979, #20171, #4655, #15259, #11642, #13330, #18731, #11528, #15471, #18841, #1736, #6694, #15031, #15141, #16823, #20068, #44, #4991, #8610, #8273, #18626, #3188, #15368, #18399, #17160, #6461, #8390, #6805, #4765, #3414, #10182, #18513, #1626, #3296, #17050, #8505 ),
 ( #3079, #10071, #16712, #9963, #1291, #16936, #9849, #2963, #10295, #5098, #13672, #1511, #22106, #21982, #13222, #13566, #20509, #6576, #21872, #8165, #13446, #20286, #20401, #4882, #11761, #22214, #11867, #12534, #14235, #272, #16024, #7142, #21069, #1835, #13786, #14008, #20625, #5209, #5658, #7027, #17600, #10735, #12198, #12425, #3522, #12092, #13901, #19382, #3963, #19054, #10839, #10402, #383, #18947, #19278, #2279, #20844, #10510, #3629, #14123, #5427, #17713, #9162, #20958, #20736, #17375, #1951, #6916, #12310, #5316, #19165, #8713, #17262, #2167, #15580, #158, #8829, #15695, #3740, #10625, #17494, #5547, #2061, #8939, #15806, #7366, #7251, #3855, #9047, #15915, #493, #14776, #13085, #705, #7472, #21174, #2719, #6095, #12642, #12970, #17935, #6209, #7580, #2497, #4189, #19930, #2828, #19816, #18264, #21282, #9378, #4402, #9708, #16131, #4078, #5875, #600, #4516, #14671, #11396, #2388, #19602, #1039, #7694, #14563, #21617, #12864, #11172, #14342, #5762, #14447, #19491, #10953, #9602, #11284, #17826, #18154, #16237, #9273, #12754, #815, #11065, #21398, #5990, #16464, #19708, #4293, #18041, #7913, #2610, #9490, #16352, #927, #7806, #21506, #8361, #15232, #16908, #10156, #11614, #6322, #1149, #20143, #3163, #1484, #16683, #13419, #20041, #6433, #4628, #20259, #13196, #14891, #6778, #8479, #17026, #21954, #4855, #21841, #18816, #11732, #1601, #4736, #18371, #21731, #3388, #9935, #18600, #1262, #8248, #13537, #10047, #22190, #15342, #16797, #16568, #1372, #13647, #11502, #8026, #15116, #2933, #9821, #20483, #8138, #4966, #20374, #13302, #22077, #15003, #18486, #3048, #5074, #11952, #6546, #6666, #11843, #18708, #3271, #15784, #5636, #3606, #13874, #134, #17469, #1927, #14211, #17579, #2040, #10376, #20713, #7002, #2146, #17348, #1810, #8807, #5184, #19, #14097, #13759, #15449, #20598, #12067, #5294, #7118, #19029, #8917, #12401, #10714, #20822, #12175, #10483, #20935, #362, #7230, #18924, #5523, #12512, #15670, #249, #15889, #21046, #7344, #13984, #9026, #10600, #5400, #6889, #19361, #10270, #8687, #467, #12285, #17136, #17239, #1711, #19136, #15553, #3717, #19253, #8586, #3499, #3832, #14751, #19686, #5740, #5850, #7557, #10818, #13060, #18017, #21592, #14426, #9356, #16216, #6074, #2256, #7890, #19464, #21376, #19792, #17801, #16441, #903, #9250, #14649, #9466, #7783, #16326, #21259, #12732, #19577, #1014, #7669, #6183, #5967, #4165, #12619, #790, #11044, #11151, #7451, #683, #21481, #17910, #2368, #9578, #4053, #3942, #17687, #18128, #2584, #9138, #16001, #2475, #10929 ),
 ( #16110, #14539, #12843, #576, #14319, #12947, #21152, #4272, #4375, #11259, #2696, #13172, #1122, #18346, #15320, #16997, #11705, #18576, #20233, #13509, #14979, #9684, #4495, #1239, #6520, #4827, #20017, #16772, #7999, #4604, #13390, #1350, #8332, #16544, #14864, #11479, #2804, #2908, #19905, #15093, #3138, #21930, #10020, #18684, #1577, #22166, #21706, #11818, #8114, #6299, #8222, #16883, #4942, #10130, #11588, #8450, #22049, #20346, #1458, #21819, #20121, #15203, #6638, #3246, #9793, #6754, #11374, #4709, #6409, #18242, #16657, #13279, #18460, #3023, #9911, #3888, #18793, #17858, #16165, #12347, #12675, #2094, #19524, #20878, #5049, #15947, #19199, #14042, #19411, #11925, #735, #4110, #2421, #7401, #15729, #15837, #17527, #20460, #13624, #5688, #9304, #8973, #19310, #10767, #16061, #3360, #10242, #7177, #9081, #7507, #5464, #10989, #10871, #3779, #2311, #3995, #17747, #9196, #413, #7288, #14158, #17110, #17632, #1688, #523, #20994, #307, #2199, #5584, #21102, #8561, #10661, #631, #12464, #14270, #12566, #14374, #21208, #5795, #21762, #21648, #9850, #12787, #6125, #845, #14805, #21534, #18184, #18402, #8057, #2641, #19633, #13115, #7834, #12999, #4217, #7723, #14594, #11203, #19740, #14922, #14700, #21429, #19845, #2529, #11097, #11424, #17965, #9406, #16270, #6019, #4320, #4432, #16381, #6241, #13223, #12892, #18069, #6351, #11314, #2747, #20069, #9628, #16490, #4656, #11529, #9521, #14479, #5910, #9736, #19961, #960, #4548, #1067, #2964, #7941, #18293, #2852, #16715, #7611, #16598, #21313, #1179, #3189, #13673, #18948, #16824, #4767, #21984, #3524, #20626, #15369, #22216, #1628, #17161, #18627, #13331, #8166, #4883, #10183, #8506, #1401, #20403, #11643, #13448, #18515, #4992, #20173, #21873, #13787, #15472, #1738, #6695, #11868, #6577, #10404, #18732, #8612, #11763, #3081, #6462, #1292, #16937, #3298, #8274, #15260, #20510, #17051, #6918, #45, #1513, #15032, #8391, #5211, #9964, #15142, #22108, #20288, #10072, #12093, #13567, #11980, #5100, #6807, #18842, #3416, #10296, #17377, #16027, #9164, #275, #21178, #13903, #10738, #8715, #495, #12645, #10627, #20847, #7145, #2171, #8943, #5764, #2281, #9049, #15808, #160, #1953, #8831, #17603, #20961, #5660, #20738, #5319, #15698, #7030, #14010, #17265, #12427, #3857, #19280, #15917, #602, #19493, #4080, #12200, #7474, #5429, #19056, #14125, #7369, #14345, #1837, #385, #15582, #19384, #17715, #5549, #12313, #17496, #12537, #14237, #21071, #3632, #3967, #10512, #2063, #19167, #3742, #7253, #10841, #9275, #12756, #14449, #707, #10955 ),
 ( #17828, #7582, #2391, #16134, #21284, #19605, #5878, #13705, #15170, #15398, #6490, #15062, #9993, #8639, #1765, #22014, #13821, #13358, #3329, #1323, #22245, #5241, #3218, #13478, #6609, #17081, #1542, #20659, #17188, #1659, #16855, #20317, #4913, #15500, #16965, #1431, #8421, #4799, #21902, #20541, #20203, #11675, #18545, #3112, #11791, #6727, #18658, #8533, #78, #8304, #10102, #10325, #15289, #22138, #6949, #13595, #20433, #12122, #18978, #5022, #16743, #8194, #12012, #6836, #11898, #5129, #18760, #9878, #10213, #18870, #3445, #14268, #9080, #521, #15945, #20877, #5463, #12345, #16060, #7287, #630, #20992, #19197, #5349, #412, #3778, #10766, #7064, #306, #7400, #10660, #17413, #9195, #3659, #7506, #14373, #17745, #17631, #5794, #8752, #2093, #19084, #2198, #17526, #14156, #21207, #3994, #8971, #15613, #21101, #15836, #5583, #194, #10543, #1984, #19309, #12462, #5687, #13933, #20768, #8864, #12232, #15728, #3557, #3887, #12565, #19410, #10870, #2310, #12674, #10435, #7176, #17295, #14041, #1870, #16380, #18183, #4547, #9734, #11201, #8055, #21647, #19960, #7833, #843, #19739, #7940, #2746, #4431, #14478, #11313, #14920, #4319, #14593, #2851, #21761, #16596, #16269, #11423, #19844, #9519, #2420, #1178, #6350, #17964, #18292, #7721, #19522, #4216, #10988, #21533, #2528, #19632, #9627, #17857, #4108, #9303, #16164, #12997, #21311, #21428, #6017, #734, #7610, #16489, #5908, #12891, #2639, #958, #6239, #12786, #11096, #9405, #14699, #13113, #18068, #14803, #1066, #6124, #19020, #13527, #10474, #11944, #8680, #18702, #10040, #13409, #17338, #1593, #18808, #15224, #22183, #5176, #3379, #13865, #15544, #8470, #8242, #15336, #125, #3155, #15110, #6772, #21947, #6539, #6993, #8353, #18916, #12058, #20367, #13751, #4847, #20252, #22068, #20706, #5284, #4958, #12164, #11724, #1704, #18593, #20590, #3597, #13641, #11836, #3265, #15442, #20476, #16901, #1477, #12, #6658, #10149, #17018, #5068, #10260, #17128, #8577, #6881, #3492, #10368, #17231, #1803, #5390, #12274, #20924, #21038, #10705, #9128, #7549, #3707, #5513, #2357, #9015, #15880, #16102, #14202, #12505, #673, #14417, #2029, #8798, #240, #4041, #7443, #13973, #14310, #19242, #21249, #8908, #3823, #12392, #5841, #4155, #21143, #19568, #353, #17569, #5730, #11035, #17459, #19126, #7221, #1917, #12721, #15990, #567, #2246, #17792, #2138, #20813, #15659, #457, #10809, #12610, #15774, #5627, #10589, #14086, #7334, #19352, #3934, #7109, #17675, #19454, #10920, #9242, #2793, #1230, #19677, #14641, #18338, #2688, #9570, #9782, #7882 ) ),
 .UNSPECIFIED., .T., .F., .F. ) 
 B_SPLINE_SURFACE_WITH_KNOTS ( ( 4, 3, 4 ),
 ( 4, 2, 2, 2, 2, 2, 2, 2, 2, 2, 2, 2, 2, 2, 2, 2, 2, 2, 2, 2, 2, 2, 2, 2, 2, 2, 2, 2, 2, 2, 2, 2, 2, 2, 2, 2, 2, 2, 2, 2, 2, 2, 2, 2, 2, 2, 2, 2, 2, 2, 2, 2, 2, 2, 2, 2, 2, 2, 2, 2, 2, 2, 2, 2, 2, 2, 2, 2, 2, 2, 2, 2, 2, 2, 2, 2, 2, 2, 2, 2, 2, 2, 2, 2, 2, 2, 2, 2, 2, 2, 2, 2, 2, 2, 2, 2, 2, 2, 2, 2, 2, 2, 2, 2, 2, 2, 2, 2, 2, 2, 2, 2, 2, 2, 2, 2, 2, 2, 2, 2, 2, 2, 2, 2, 2, 2, 2, 2, 2, 2, 2, 2, 2, 2, 2, 2, 2, 2, 2, 2, 2, 2, 2, 2, 2, 2, 2, 2, 2, 2, 2, 2, 2, 2, 2, 2, 2, 2, 2, 2, 2, 2, 2, 2, 2, 2, 2, 4 ),
 ( 0.000000000000000000, 0.5000000000000000000, 1.000000000000000000 ),
 ( 0.000000000000000000, 0.001952908952989333875, 0.003905817905978667751, 0.007323408573709997045, 0.01074099924144132634, 0.01415858990917265650, 0.01586738524303832332, 0.01757618057690398666, 0.02099377124463531682, 0.02441136191236664699, 0.02782895258009797368, 0.03124654324782930384, 0.03466413391556063400, 0.03808172458329196070, 0.04149931525102329433, 0.04491690591875462102, 0.04662570125262028436, 0.04833449658648594771, 0.05175208725421727440, 0.05346088258808293775, 0.05516967792194860110, 0.05858726858967993473, 0.06200485925741126836, 0.06542244992514259505, 0.06884004059287393562, 0.07225763126060526231, 0.07567522192833658901, 0.07909281259606792958, 0.08251040326379925627, 0.08421919859766491268, 0.08592799393153058296, 0.08934558459926195129, 0.09276317526699331961, 0.09447197060085900377, 0.09618076593472468794, 0.09959835660245604239, 0.1030159472701873968, 0.1064335379379187652, 0.1098511286056501335, 0.1132687192733815018, 0.1166863099411127869, 0.1201039006088440858, 0.1235214912765753847, 0.1252302866104410273, 0.1269390819443066698, 0.1303566726120379826, 0.1320654679459036251, 0.1337742632797692677, 0.1371918539475005527, 0.1406094446152318378, 0.1440270352829631784, 0.1474446259506944912, 0.1508622166184258040, 0.1542798072861571446, 0.1576973979538884851, 0.1611149886216198257, 0.1645325792893511663, 0.1679501699570824791, 0.1713677606248137919, 0.1747853512925451325, 0.1764941466264108028, 0.1782029419602764730, 0.1816205326280078136, 0.1850381232957391542, 0.1884557139634704670, 0.1918733046312017798, 0.1952908952989331204, 0.1987084859666644610, 0.2021260766343957738, 0.2055436673021270866, 0.2072524626359927569, 0.2089612579698584272, 0.2123788486375897677, 0.2140876439714554380, 0.2157964393053211083, 0.2192140299730524489, 0.2226316206407837617, 0.2260492113085151300, 0.2294668019762464706, 0.2328843926439778111, 0.2363019833117091517, 0.2397195739794404923, 0.2431371646471718329, 0.2465547553149031734, 0.2499723459826345140, 0.2533899366503657991, 0.2568075273180971396, 0.2602251179858284802, 0.2636427086535597653, 0.2670602993212910503, 0.2704778899890223909, 0.2738954806567537315, 0.2773130713244850165, 0.2807306619922163571, 0.2841482526599476977, 0.2858570479938133957, 0.2875658433276790382, 0.2909834339954103788, 0.2926922293292760768, 0.2944010246631417194, 0.2978186153308730599, 0.3012362059986043450, 0.3046537966663356856, 0.3080713873340670261, 0.3114889780017983112, 0.3149065686695296518, 0.3183241593372609923, 0.3217417500049923329, 0.3234505453388579754, 0.3251593406727236735, 0.3285769313404549585, 0.3319945220081862991, 0.3354121126759176397, 0.3388297033436489247, 0.3422472940113802653, 0.3456648846791116059, 0.3490824753468429464, 0.3525000660145742870, 0.3559176566823056276, 0.3593352473500369682, 0.3627528380177683087, 0.3661704286854996493, 0.3695880193532309343, 0.3730056100209622749, 0.3747144053548279174, 0.3764232006886936155, 0.3798407913564249005, 0.3832583820241562411, 0.3866759726918875817, 0.3900935633596189223, 0.3935111540273502628, 0.3969287446950816034, 0.4003463353628129440, 0.4037639260305442845, 0.4054727213644099271, 0.4071815166982756251, 0.4105991073660069102, 0.4140166980337382507, 0.4157254933676038933, 0.4174342887014695913, 0.4208518793692008764, 0.4242694700369322169, 0.4276870607046635575, 0.4311046513723948981, 0.4345222420401262386, 0.4379398327078575237, 0.4413574233755888643, 0.4447750140433202048, 0.4464838093771859029, 0.4481926047110515454, 0.4516101953787828860, 0.4533189907126485840, 0.4550277860465142266, 0.4584453767142455671, 0.4618629673819769077, 0.4652805580497082483, 0.4686981487174395888, 0.4721157393851709294, 0.4755333300529022145, 0.4789509207206335550, 0.4823685113883648956, 0.4840773067222305381, 0.4857861020560961807, 0.4892036927238275212, 0.4926212833915588618, 0.4960388740592901469, 0.4979917830122794764, 0.4999446919652688059 ),
 .UNSPECIFIED. ) 
 GEOMETRIC_REPRESENTATION_ITEM ( )  RATIONAL_B_SPLINE_SURFACE ( (
 ( 1.000000000000000000, 1.000000000000000000, 1.000000000000000000, 1.000000000000000000, 1.000000000000000000, 1.000000000000000000, 1.000000000000000000, 1.000000000000000000, 1.000000000000000000, 1.000000000000000000, 1.000000000000000000, 1.000000000000000000, 1.000000000000000000, 1.000000000000000000, 1.000000000000000000, 1.000000000000000000, 1.000000000000000000, 1.000000000000000000, 1.000000000000000000, 1.000000000000000000, 1.000000000000000000, 1.000000000000000000, 1.000000000000000000, 1.000000000000000000, 1.000000000000000000, 1.000000000000000000, 1.000000000000000000, 1.000000000000000000, 1.000000000000000000, 1.000000000000000000, 1.000000000000000000, 1.000000000000000000, 1.000000000000000000, 1.000000000000000000, 1.000000000000000000, 1.000000000000000000, 1.000000000000000000, 1.000000000000000000, 1.000000000000000000, 1.000000000000000000, 1.000000000000000000, 1.000000000000000000, 1.000000000000000000, 1.000000000000000000, 1.000000000000000000, 1.000000000000000000, 1.000000000000000000, 1.000000000000000000, 1.000000000000000000, 1.000000000000000000, 1.000000000000000000, 1.000000000000000000, 1.000000000000000000, 1.000000000000000000, 1.000000000000000000, 1.000000000000000000, 1.000000000000000000, 1.000000000000000000, 1.000000000000000000, 1.000000000000000000, 1.000000000000000000, 1.000000000000000000, 1.000000000000000000, 1.000000000000000000, 1.000000000000000000, 1.000000000000000000, 1.000000000000000000, 1.000000000000000000, 1.000000000000000000, 1.000000000000000000, 1.000000000000000000, 1.000000000000000000, 1.000000000000000000, 1.000000000000000000, 1.000000000000000000, 1.000000000000000000, 1.000000000000000000, 1.000000000000000000, 1.000000000000000000, 1.000000000000000000, 1.000000000000000000, 1.000000000000000000, 1.000000000000000000, 1.000000000000000000, 1.000000000000000000, 1.000000000000000000, 1.000000000000000000, 1.000000000000000000, 1.000000000000000000, 1.000000000000000000, 1.000000000000000000, 1.000000000000000000, 1.000000000000000000, 1.000000000000000000, 1.000000000000000000, 1.000000000000000000, 1.000000000000000000, 1.000000000000000000, 1.000000000000000000, 1.000000000000000000, 1.000000000000000000, 1.000000000000000000, 1.000000000000000000, 1.000000000000000000, 1.000000000000000000, 1.000000000000000000, 1.000000000000000000, 1.000000000000000000, 1.000000000000000000, 1.000000000000000000, 1.000000000000000000, 1.000000000000000000, 1.000000000000000000, 1.000000000000000000, 1.000000000000000000, 1.000000000000000000, 1.000000000000000000, 1.000000000000000000, 1.000000000000000000, 1.000000000000000000, 1.000000000000000000, 1.000000000000000000, 1.000000000000000000, 1.000000000000000000, 1.000000000000000000, 1.000000000000000000, 1.000000000000000000, 1.000000000000000000, 1.000000000000000000, 1.000000000000000000, 1.000000000000000000, 1.000000000000000000, 1.000000000000000000, 1.000000000000000000, 1.000000000000000000, 1.000000000000000000, 1.000000000000000000, 1.000000000000000000, 1.000000000000000000, 1.000000000000000000, 1.000000000000000000, 1.000000000000000000, 1.000000000000000000, 1.000000000000000000, 1.000000000000000000, 1.000000000000000000, 1.000000000000000000, 1.000000000000000000, 1.000000000000000000, 1.000000000000000000, 1.000000000000000000, 1.000000000000000000, 1.000000000000000000, 1.000000000000000000, 1.000000000000000000, 1.000000000000000000, 1.000000000000000000, 1.000000000000000000, 1.000000000000000000, 1.000000000000000000, 1.000000000000000000, 1.000000000000000000, 1.000000000000000000, 1.000000000000000000, 1.000000000000000000, 1.000000000000000000, 1.000000000000000000, 1.000000000000000000, 1.000000000000000000, 1.000000000000000000, 1.000000000000000000, 1.000000000000000000, 1.000000000000000000, 1.000000000000000000, 1.000000000000000000, 1.000000000000000000, 1.000000000000000000, 1.000000000000000000, 1.000000000000000000, 1.000000000000000000, 1.000000000000000000, 1.000000000000000000, 1.000000000000000000, 1.000000000000000000, 1.000000000000000000, 1.000000000000000000, 1.000000000000000000, 1.000000000000000000, 1.000000000000000000, 1.000000000000000000, 1.000000000000000000, 1.000000000000000000, 1.000000000000000000, 1.000000000000000000, 1.000000000000000000, 1.000000000000000000, 1.000000000000000000, 1.000000000000000000, 1.000000000000000000, 1.000000000000000000, 1.000000000000000000, 1.000000000000000000, 1.000000000000000000, 1.000000000000000000, 1.000000000000000000, 1.000000000000000000, 1.000000000000000000, 1.000000000000000000, 1.000000000000000000, 1.000000000000000000, 1.000000000000000000, 1.000000000000000000, 1.000000000000000000, 1.000000000000000000, 1.000000000000000000, 1.000000000000000000, 1.000000000000000000, 1.000000000000000000, 1.000000000000000000, 1.000000000000000000, 1.000000000000000000, 1.000000000000000000, 1.000000000000000000, 1.000000000000000000, 1.000000000000000000, 1.000000000000000000, 1.000000000000000000, 1.000000000000000000, 1.000000000000000000, 1.000000000000000000, 1.000000000000000000, 1.000000000000000000, 1.000000000000000000, 1.000000000000000000, 1.000000000000000000, 1.000000000000000000, 1.000000000000000000, 1.000000000000000000, 1.000000000000000000, 1.000000000000000000, 1.000000000000000000, 1.000000000000000000, 1.000000000000000000, 1.000000000000000000, 1.000000000000000000, 1.000000000000000000, 1.000000000000000000, 1.000000000000000000, 1.000000000000000000, 1.000000000000000000, 1.000000000000000000, 1.000000000000000000, 1.000000000000000000, 1.000000000000000000, 1.000000000000000000, 1.000000000000000000, 1.000000000000000000, 1.000000000000000000, 1.000000000000000000, 1.000000000000000000, 1.000000000000000000, 1.000000000000000000, 1.000000000000000000, 1.000000000000000000, 1.000000000000000000, 1.000000000000000000, 1.000000000000000000, 1.000000000000000000, 1.000000000000000000, 1.000000000000000000, 1.000000000000000000, 1.000000000000000000, 1.000000000000000000, 1.000000000000000000, 1.000000000000000000, 1.000000000000000000, 1.000000000000000000, 1.000000000000000000, 1.000000000000000000, 1.000000000000000000, 1.000000000000000000, 1.000000000000000000, 1.000000000000000000, 1.000000000000000000, 1.000000000000000000, 1.000000000000000000, 1.000000000000000000, 1.000000000000000000, 1.000000000000000000, 1.000000000000000000, 1.000000000000000000, 1.000000000000000000, 1.000000000000000000, 1.000000000000000000, 1.000000000000000000, 1.000000000000000000, 1.000000000000000000, 1.000000000000000000, 1.000000000000000000, 1.000000000000000000, 1.000000000000000000, 1.000000000000000000, 1.000000000000000000, 1.000000000000000000, 1.000000000000000000, 1.000000000000000000, 1.000000000000000000, 1.000000000000000000, 1.000000000000000000, 1.000000000000000000, 1.000000000000000000, 1.000000000000000000, 1.000000000000000000, 1.000000000000000000, 1.000000000000000000, 1.000000000000000000, 1.000000000000000000, 1.000000000000000000, 1.000000000000000000, 1.000000000000000000, 1.000000000000000000, 1.000000000000000000, 1.000000000000000000, 1.000000000000000000, 1.000000000000000000, 1.000000000000000000, 1.000000000000000000, 1.000000000000000000, 1.000000000000000000, 1.000000000000000000, 1.000000000000000000, 1.000000000000000000, 1.000000000000000000, 1.000000000000000000, 1.000000000000000000, 1.000000000000000000),
 ( 0.3333333333333333703, 0.3333333333333333703, 0.3333333333333333703, 0.3333333333333333703, 0.3333333333333333703, 0.3333333333333333703, 0.3333333333333333703, 0.3333333333333333703, 0.3333333333333333703, 0.3333333333333333703, 0.3333333333333333703, 0.3333333333333333703, 0.3333333333333333703, 0.3333333333333333703, 0.3333333333333333703, 0.3333333333333333703, 0.3333333333333333703, 0.3333333333333333703, 0.3333333333333333703, 0.3333333333333333703, 0.3333333333333333703, 0.3333333333333333703, 0.3333333333333333703, 0.3333333333333333703, 0.3333333333333333703, 0.3333333333333333703, 0.3333333333333333703, 0.3333333333333333703, 0.3333333333333333703, 0.3333333333333333703, 0.3333333333333333703, 0.3333333333333333703, 0.3333333333333333703, 0.3333333333333333703, 0.3333333333333333703, 0.3333333333333333703, 0.3333333333333333703, 0.3333333333333333703, 0.3333333333333333703, 0.3333333333333333703, 0.3333333333333333703, 0.3333333333333333703, 0.3333333333333333703, 0.3333333333333333703, 0.3333333333333333703, 0.3333333333333333703, 0.3333333333333333703, 0.3333333333333333703, 0.3333333333333333703, 0.3333333333333333703, 0.3333333333333333703, 0.3333333333333333703, 0.3333333333333333703, 0.3333333333333333703, 0.3333333333333333703, 0.3333333333333333703, 0.3333333333333333703, 0.3333333333333333703, 0.3333333333333333703, 0.3333333333333333703, 0.3333333333333333703, 0.3333333333333333703, 0.3333333333333333703, 0.3333333333333333703, 0.3333333333333333703, 0.3333333333333333703, 0.3333333333333333703, 0.3333333333333333703, 0.3333333333333333703, 0.3333333333333333703, 0.3333333333333333703, 0.3333333333333333703, 0.3333333333333333703, 0.3333333333333333703, 0.3333333333333333703, 0.3333333333333333703, 0.3333333333333333703, 0.3333333333333333703, 0.3333333333333333703, 0.3333333333333333703, 0.3333333333333333703, 0.3333333333333333703, 0.3333333333333333703, 0.3333333333333333703, 0.3333333333333333703, 0.3333333333333333703, 0.3333333333333333703, 0.3333333333333333703, 0.3333333333333333703, 0.3333333333333333703, 0.3333333333333333703, 0.3333333333333333703, 0.3333333333333333703, 0.3333333333333333703, 0.3333333333333333703, 0.3333333333333333703, 0.3333333333333333703, 0.3333333333333333703, 0.3333333333333333703, 0.3333333333333333703, 0.3333333333333333703, 0.3333333333333333703, 0.3333333333333333703, 0.3333333333333333703, 0.3333333333333333703, 0.3333333333333333703, 0.3333333333333333703, 0.3333333333333333703, 0.3333333333333333703, 0.3333333333333333703, 0.3333333333333333703, 0.3333333333333333703, 0.3333333333333333703, 0.3333333333333333703, 0.3333333333333333703, 0.3333333333333333703, 0.3333333333333333703, 0.3333333333333333703, 0.3333333333333333703, 0.3333333333333333703, 0.3333333333333333703, 0.3333333333333333703, 0.3333333333333333703, 0.3333333333333333703, 0.3333333333333333703, 0.3333333333333333703, 0.3333333333333333703, 0.3333333333333333703, 0.3333333333333333703, 0.3333333333333333703, 0.3333333333333333703, 0.3333333333333333703, 0.3333333333333333703, 0.3333333333333333703, 0.3333333333333333703, 0.3333333333333333703, 0.3333333333333333703, 0.3333333333333333703, 0.3333333333333333703, 0.3333333333333333703, 0.3333333333333333703, 0.3333333333333333703, 0.3333333333333333703, 0.3333333333333333703, 0.3333333333333333703, 0.3333333333333333703, 0.3333333333333333703, 0.3333333333333333703, 0.3333333333333333703, 0.3333333333333333703, 0.3333333333333333703, 0.3333333333333333703, 0.3333333333333333703, 0.3333333333333333703, 0.3333333333333333703, 0.3333333333333333703, 0.3333333333333333703, 0.3333333333333333703, 0.3333333333333333703, 0.3333333333333333703, 0.3333333333333333703, 0.3333333333333333703, 0.3333333333333333703, 0.3333333333333333703, 0.3333333333333333703, 0.3333333333333333703, 0.3333333333333333703, 0.3333333333333333703, 0.3333333333333333703, 0.3333333333333333703, 0.3333333333333333703, 0.3333333333333333703, 0.3333333333333333703, 0.3333333333333333703, 0.3333333333333333703, 0.3333333333333333703, 0.3333333333333333703, 0.3333333333333333703, 0.3333333333333333703, 0.3333333333333333703, 0.3333333333333333703, 0.3333333333333333703, 0.3333333333333333703, 0.3333333333333333703, 0.3333333333333333703, 0.3333333333333333703, 0.3333333333333333703, 0.3333333333333333703, 0.3333333333333333703, 0.3333333333333333703, 0.3333333333333333703, 0.3333333333333333703, 0.3333333333333333703, 0.3333333333333333703, 0.3333333333333333703, 0.3333333333333333703, 0.3333333333333333703, 0.3333333333333333703, 0.3333333333333333703, 0.3333333333333333703, 0.3333333333333333703, 0.3333333333333333703, 0.3333333333333333703, 0.3333333333333333703, 0.3333333333333333703, 0.3333333333333333703, 0.3333333333333333703, 0.3333333333333333703, 0.3333333333333333703, 0.3333333333333333703, 0.3333333333333333703, 0.3333333333333333703, 0.3333333333333333703, 0.3333333333333333703, 0.3333333333333333703, 0.3333333333333333703, 0.3333333333333333703, 0.3333333333333333703, 0.3333333333333333703, 0.3333333333333333703, 0.3333333333333333703, 0.3333333333333333703, 0.3333333333333333703, 0.3333333333333333703, 0.3333333333333333703, 0.3333333333333333703, 0.3333333333333333703, 0.3333333333333333703, 0.3333333333333333703, 0.3333333333333333703, 0.3333333333333333703, 0.3333333333333333703, 0.3333333333333333703, 0.3333333333333333703, 0.3333333333333333703, 0.3333333333333333703, 0.3333333333333333703, 0.3333333333333333703, 0.3333333333333333703, 0.3333333333333333703, 0.3333333333333333703, 0.3333333333333333703, 0.3333333333333333703, 0.3333333333333333703, 0.3333333333333333703, 0.3333333333333333703, 0.3333333333333333703, 0.3333333333333333703, 0.3333333333333333703, 0.3333333333333333703, 0.3333333333333333703, 0.3333333333333333703, 0.3333333333333333703, 0.3333333333333333703, 0.3333333333333333703, 0.3333333333333333703, 0.3333333333333333703, 0.3333333333333333703, 0.3333333333333333703, 0.3333333333333333703, 0.3333333333333333703, 0.3333333333333333703, 0.3333333333333333703, 0.3333333333333333703, 0.3333333333333333703, 0.3333333333333333703, 0.3333333333333333703, 0.3333333333333333703, 0.3333333333333333703, 0.3333333333333333703, 0.3333333333333333703, 0.3333333333333333703, 0.3333333333333333703, 0.3333333333333333703, 0.3333333333333333703, 0.3333333333333333703, 0.3333333333333333703, 0.3333333333333333703, 0.3333333333333333703, 0.3333333333333333703, 0.3333333333333333703, 0.3333333333333333703, 0.3333333333333333703, 0.3333333333333333703, 0.3333333333333333703, 0.3333333333333333703, 0.3333333333333333703, 0.3333333333333333703, 0.3333333333333333703, 0.3333333333333333703, 0.3333333333333333703, 0.3333333333333333703, 0.3333333333333333703, 0.3333333333333333703, 0.3333333333333333703, 0.3333333333333333703, 0.3333333333333333703, 0.3333333333333333703, 0.3333333333333333703, 0.3333333333333333703, 0.3333333333333333703, 0.3333333333333333703, 0.3333333333333333703, 0.3333333333333333703, 0.3333333333333333703, 0.3333333333333333703, 0.3333333333333333703, 0.3333333333333333703, 0.3333333333333333703, 0.3333333333333333703, 0.3333333333333333703, 0.3333333333333333703, 0.3333333333333333703, 0.3333333333333333703, 0.3333333333333333703, 0.3333333333333333703, 0.3333333333333333703, 0.3333333333333333703, 0.3333333333333333703, 0.3333333333333333703, 0.3333333333333333703, 0.3333333333333333703, 0.3333333333333333703, 0.3333333333333333703, 0.3333333333333333703, 0.3333333333333333703, 0.3333333333333333703, 0.3333333333333333703, 0.3333333333333333703, 0.3333333333333333703, 0.3333333333333333703, 0.3333333333333333703, 0.3333333333333333703, 0.3333333333333333703, 0.3333333333333333703, 0.3333333333333333703),
 ( 0.3333333333333333703, 0.3333333333333333703, 0.3333333333333333703, 0.3333333333333333703, 0.3333333333333333703, 0.3333333333333333703, 0.3333333333333333703, 0.3333333333333333703, 0.3333333333333333703, 0.3333333333333333703, 0.3333333333333333703, 0.3333333333333333703, 0.3333333333333333703, 0.3333333333333333703, 0.3333333333333333703, 0.3333333333333333703, 0.3333333333333333703, 0.3333333333333333703, 0.3333333333333333703, 0.3333333333333333703, 0.3333333333333333703, 0.3333333333333333703, 0.3333333333333333703, 0.3333333333333333703, 0.3333333333333333703, 0.3333333333333333703, 0.3333333333333333703, 0.3333333333333333703, 0.3333333333333333703, 0.3333333333333333703, 0.3333333333333333703, 0.3333333333333333703, 0.3333333333333333703, 0.3333333333333333703, 0.3333333333333333703, 0.3333333333333333703, 0.3333333333333333703, 0.3333333333333333703, 0.3333333333333333703, 0.3333333333333333703, 0.3333333333333333703, 0.3333333333333333703, 0.3333333333333333703, 0.3333333333333333703, 0.3333333333333333703, 0.3333333333333333703, 0.3333333333333333703, 0.3333333333333333703, 0.3333333333333333703, 0.3333333333333333703, 0.3333333333333333703, 0.3333333333333333703, 0.3333333333333333703, 0.3333333333333333703, 0.3333333333333333703, 0.3333333333333333703, 0.3333333333333333703, 0.3333333333333333703, 0.3333333333333333703, 0.3333333333333333703, 0.3333333333333333703, 0.3333333333333333703, 0.3333333333333333703, 0.3333333333333333703, 0.3333333333333333703, 0.3333333333333333703, 0.3333333333333333703, 0.3333333333333333703, 0.3333333333333333703, 0.3333333333333333703, 0.3333333333333333703, 0.3333333333333333703, 0.3333333333333333703, 0.3333333333333333703, 0.3333333333333333703, 0.3333333333333333703, 0.3333333333333333703, 0.3333333333333333703, 0.3333333333333333703, 0.3333333333333333703, 0.3333333333333333703, 0.3333333333333333703, 0.3333333333333333703, 0.3333333333333333703, 0.3333333333333333703, 0.3333333333333333703, 0.3333333333333333703, 0.3333333333333333703, 0.3333333333333333703, 0.3333333333333333703, 0.3333333333333333703, 0.3333333333333333703, 0.3333333333333333703, 0.3333333333333333703, 0.3333333333333333703, 0.3333333333333333703, 0.3333333333333333703, 0.3333333333333333703, 0.3333333333333333703, 0.3333333333333333703, 0.3333333333333333703, 0.3333333333333333703, 0.3333333333333333703, 0.3333333333333333703, 0.3333333333333333703, 0.3333333333333333703, 0.3333333333333333703, 0.3333333333333333703, 0.3333333333333333703, 0.3333333333333333703, 0.3333333333333333703, 0.3333333333333333703, 0.3333333333333333703, 0.3333333333333333703, 0.3333333333333333703, 0.3333333333333333703, 0.3333333333333333703, 0.3333333333333333703, 0.3333333333333333703, 0.3333333333333333703, 0.3333333333333333703, 0.3333333333333333703, 0.3333333333333333703, 0.3333333333333333703, 0.3333333333333333703, 0.3333333333333333703, 0.3333333333333333703, 0.3333333333333333703, 0.3333333333333333703, 0.3333333333333333703, 0.3333333333333333703, 0.3333333333333333703, 0.3333333333333333703, 0.3333333333333333703, 0.3333333333333333703, 0.3333333333333333703, 0.3333333333333333703, 0.3333333333333333703, 0.3333333333333333703, 0.3333333333333333703, 0.3333333333333333703, 0.3333333333333333703, 0.3333333333333333703, 0.3333333333333333703, 0.3333333333333333703, 0.3333333333333333703, 0.3333333333333333703, 0.3333333333333333703, 0.3333333333333333703, 0.3333333333333333703, 0.3333333333333333703, 0.3333333333333333703, 0.3333333333333333703, 0.3333333333333333703, 0.3333333333333333703, 0.3333333333333333703, 0.3333333333333333703, 0.3333333333333333703, 0.3333333333333333703, 0.3333333333333333703, 0.3333333333333333703, 0.3333333333333333703, 0.3333333333333333703, 0.3333333333333333703, 0.3333333333333333703, 0.3333333333333333703, 0.3333333333333333703, 0.3333333333333333703, 0.3333333333333333703, 0.3333333333333333703, 0.3333333333333333703, 0.3333333333333333703, 0.3333333333333333703, 0.3333333333333333703, 0.3333333333333333703, 0.3333333333333333703, 0.3333333333333333703, 0.3333333333333333703, 0.3333333333333333703, 0.3333333333333333703, 0.3333333333333333703, 0.3333333333333333703, 0.3333333333333333703, 0.3333333333333333703, 0.3333333333333333703, 0.3333333333333333703, 0.3333333333333333703, 0.3333333333333333703, 0.3333333333333333703, 0.3333333333333333703, 0.3333333333333333703, 0.3333333333333333703, 0.3333333333333333703, 0.3333333333333333703, 0.3333333333333333703, 0.3333333333333333703, 0.3333333333333333703, 0.3333333333333333703, 0.3333333333333333703, 0.3333333333333333703, 0.3333333333333333703, 0.3333333333333333703, 0.3333333333333333703, 0.3333333333333333703, 0.3333333333333333703, 0.3333333333333333703, 0.3333333333333333703, 0.3333333333333333703, 0.3333333333333333703, 0.3333333333333333703, 0.3333333333333333703, 0.3333333333333333703, 0.3333333333333333703, 0.3333333333333333703, 0.3333333333333333703, 0.3333333333333333703, 0.3333333333333333703, 0.3333333333333333703, 0.3333333333333333703, 0.3333333333333333703, 0.3333333333333333703, 0.3333333333333333703, 0.3333333333333333703, 0.3333333333333333703, 0.3333333333333333703, 0.3333333333333333703, 0.3333333333333333703, 0.3333333333333333703, 0.3333333333333333703, 0.3333333333333333703, 0.3333333333333333703, 0.3333333333333333703, 0.3333333333333333703, 0.3333333333333333703, 0.3333333333333333703, 0.3333333333333333703, 0.3333333333333333703, 0.3333333333333333703, 0.3333333333333333703, 0.3333333333333333703, 0.3333333333333333703, 0.3333333333333333703, 0.3333333333333333703, 0.3333333333333333703, 0.3333333333333333703, 0.3333333333333333703, 0.3333333333333333703, 0.3333333333333333703, 0.3333333333333333703, 0.3333333333333333703, 0.3333333333333333703, 0.3333333333333333703, 0.3333333333333333703, 0.3333333333333333703, 0.3333333333333333703, 0.3333333333333333703, 0.3333333333333333703, 0.3333333333333333703, 0.3333333333333333703, 0.3333333333333333703, 0.3333333333333333703, 0.3333333333333333703, 0.3333333333333333703, 0.3333333333333333703, 0.3333333333333333703, 0.3333333333333333703, 0.3333333333333333703, 0.3333333333333333703, 0.3333333333333333703, 0.3333333333333333703, 0.3333333333333333703, 0.3333333333333333703, 0.3333333333333333703, 0.3333333333333333703, 0.3333333333333333703, 0.3333333333333333703, 0.3333333333333333703, 0.3333333333333333703, 0.3333333333333333703, 0.3333333333333333703, 0.3333333333333333703, 0.3333333333333333703, 0.3333333333333333703, 0.3333333333333333703, 0.3333333333333333703, 0.3333333333333333703, 0.3333333333333333703, 0.3333333333333333703, 0.3333333333333333703, 0.3333333333333333703, 0.3333333333333333703, 0.3333333333333333703, 0.3333333333333333703, 0.3333333333333333703, 0.3333333333333333703, 0.3333333333333333703, 0.3333333333333333703, 0.3333333333333333703, 0.3333333333333333703, 0.3333333333333333703, 0.3333333333333333703, 0.3333333333333333703, 0.3333333333333333703, 0.3333333333333333703, 0.3333333333333333703, 0.3333333333333333703, 0.3333333333333333703, 0.3333333333333333703, 0.3333333333333333703, 0.3333333333333333703, 0.3333333333333333703, 0.3333333333333333703, 0.3333333333333333703, 0.3333333333333333703, 0.3333333333333333703, 0.3333333333333333703, 0.3333333333333333703, 0.3333333333333333703, 0.3333333333333333703, 0.3333333333333333703, 0.3333333333333333703, 0.3333333333333333703, 0.3333333333333333703, 0.3333333333333333703, 0.3333333333333333703, 0.3333333333333333703, 0.3333333333333333703, 0.3333333333333333703, 0.3333333333333333703, 0.3333333333333333703, 0.3333333333333333703, 0.3333333333333333703, 0.3333333333333333703, 0.3333333333333333703, 0.3333333333333333703, 0.3333333333333333703),
 ( 1.000000000000000000, 1.000000000000000000, 1.000000000000000000, 1.000000000000000000, 1.000000000000000000, 1.000000000000000000, 1.000000000000000000, 1.000000000000000000, 1.000000000000000000, 1.000000000000000000, 1.000000000000000000, 1.000000000000000000, 1.000000000000000000, 1.000000000000000000, 1.000000000000000000, 1.000000000000000000, 1.000000000000000000, 1.000000000000000000, 1.000000000000000000, 1.000000000000000000, 1.000000000000000000, 1.000000000000000000, 1.000000000000000000, 1.000000000000000000, 1.000000000000000000, 1.000000000000000000, 1.000000000000000000, 1.000000000000000000, 1.000000000000000000, 1.000000000000000000, 1.000000000000000000, 1.000000000000000000, 1.000000000000000000, 1.000000000000000000, 1.000000000000000000, 1.000000000000000000, 1.000000000000000000, 1.000000000000000000, 1.000000000000000000, 1.000000000000000000, 1.000000000000000000, 1.000000000000000000, 1.000000000000000000, 1.000000000000000000, 1.000000000000000000, 1.000000000000000000, 1.000000000000000000, 1.000000000000000000, 1.000000000000000000, 1.000000000000000000, 1.000000000000000000, 1.000000000000000000, 1.000000000000000000, 1.000000000000000000, 1.000000000000000000, 1.000000000000000000, 1.000000000000000000, 1.000000000000000000, 1.000000000000000000, 1.000000000000000000, 1.000000000000000000, 1.000000000000000000, 1.000000000000000000, 1.000000000000000000, 1.000000000000000000, 1.000000000000000000, 1.000000000000000000, 1.000000000000000000, 1.000000000000000000, 1.000000000000000000, 1.000000000000000000, 1.000000000000000000, 1.000000000000000000, 1.000000000000000000, 1.000000000000000000, 1.000000000000000000, 1.000000000000000000, 1.000000000000000000, 1.000000000000000000, 1.000000000000000000, 1.000000000000000000, 1.000000000000000000, 1.000000000000000000, 1.000000000000000000, 1.000000000000000000, 1.000000000000000000, 1.000000000000000000, 1.000000000000000000, 1.000000000000000000, 1.000000000000000000, 1.000000000000000000, 1.000000000000000000, 1.000000000000000000, 1.000000000000000000, 1.000000000000000000, 1.000000000000000000, 1.000000000000000000, 1.000000000000000000, 1.000000000000000000, 1.000000000000000000, 1.000000000000000000, 1.000000000000000000, 1.000000000000000000, 1.000000000000000000, 1.000000000000000000, 1.000000000000000000, 1.000000000000000000, 1.000000000000000000, 1.000000000000000000, 1.000000000000000000, 1.000000000000000000, 1.000000000000000000, 1.000000000000000000, 1.000000000000000000, 1.000000000000000000, 1.000000000000000000, 1.000000000000000000, 1.000000000000000000, 1.000000000000000000, 1.000000000000000000, 1.000000000000000000, 1.000000000000000000, 1.000000000000000000, 1.000000000000000000, 1.000000000000000000, 1.000000000000000000, 1.000000000000000000, 1.000000000000000000, 1.000000000000000000, 1.000000000000000000, 1.000000000000000000, 1.000000000000000000, 1.000000000000000000, 1.000000000000000000, 1.000000000000000000, 1.000000000000000000, 1.000000000000000000, 1.000000000000000000, 1.000000000000000000, 1.000000000000000000, 1.000000000000000000, 1.000000000000000000, 1.000000000000000000, 1.000000000000000000, 1.000000000000000000, 1.000000000000000000, 1.000000000000000000, 1.000000000000000000, 1.000000000000000000, 1.000000000000000000, 1.000000000000000000, 1.000000000000000000, 1.000000000000000000, 1.000000000000000000, 1.000000000000000000, 1.000000000000000000, 1.000000000000000000, 1.000000000000000000, 1.000000000000000000, 1.000000000000000000, 1.000000000000000000, 1.000000000000000000, 1.000000000000000000, 1.000000000000000000, 1.000000000000000000, 1.000000000000000000, 1.000000000000000000, 1.000000000000000000, 1.000000000000000000, 1.000000000000000000, 1.000000000000000000, 1.000000000000000000, 1.000000000000000000, 1.000000000000000000, 1.000000000000000000, 1.000000000000000000, 1.000000000000000000, 1.000000000000000000, 1.000000000000000000, 1.000000000000000000, 1.000000000000000000, 1.000000000000000000, 1.000000000000000000, 1.000000000000000000, 1.000000000000000000, 1.000000000000000000, 1.000000000000000000, 1.000000000000000000, 1.000000000000000000, 1.000000000000000000, 1.000000000000000000, 1.000000000000000000, 1.000000000000000000, 1.000000000000000000, 1.000000000000000000, 1.000000000000000000, 1.000000000000000000, 1.000000000000000000, 1.000000000000000000, 1.000000000000000000, 1.000000000000000000, 1.000000000000000000, 1.000000000000000000, 1.000000000000000000, 1.000000000000000000, 1.000000000000000000, 1.000000000000000000, 1.000000000000000000, 1.000000000000000000, 1.000000000000000000, 1.000000000000000000, 1.000000000000000000, 1.000000000000000000, 1.000000000000000000, 1.000000000000000000, 1.000000000000000000, 1.000000000000000000, 1.000000000000000000, 1.000000000000000000, 1.000000000000000000, 1.000000000000000000, 1.000000000000000000, 1.000000000000000000, 1.000000000000000000, 1.000000000000000000, 1.000000000000000000, 1.000000000000000000, 1.000000000000000000, 1.000000000000000000, 1.000000000000000000, 1.000000000000000000, 1.000000000000000000, 1.000000000000000000, 1.000000000000000000, 1.000000000000000000, 1.000000000000000000, 1.000000000000000000, 1.000000000000000000, 1.000000000000000000, 1.000000000000000000, 1.000000000000000000, 1.000000000000000000, 1.000000000000000000, 1.000000000000000000, 1.000000000000000000, 1.000000000000000000, 1.000000000000000000, 1.000000000000000000, 1.000000000000000000, 1.000000000000000000, 1.000000000000000000, 1.000000000000000000, 1.000000000000000000, 1.000000000000000000, 1.000000000000000000, 1.000000000000000000, 1.000000000000000000, 1.000000000000000000, 1.000000000000000000, 1.000000000000000000, 1.000000000000000000, 1.000000000000000000, 1.000000000000000000, 1.000000000000000000, 1.000000000000000000, 1.000000000000000000, 1.000000000000000000, 1.000000000000000000, 1.000000000000000000, 1.000000000000000000, 1.000000000000000000, 1.000000000000000000, 1.000000000000000000, 1.000000000000000000, 1.000000000000000000, 1.000000000000000000, 1.000000000000000000, 1.000000000000000000, 1.000000000000000000, 1.000000000000000000, 1.000000000000000000, 1.000000000000000000, 1.000000000000000000, 1.000000000000000000, 1.000000000000000000, 1.000000000000000000, 1.000000000000000000, 1.000000000000000000, 1.000000000000000000, 1.000000000000000000, 1.000000000000000000, 1.000000000000000000, 1.000000000000000000, 1.000000000000000000, 1.000000000000000000, 1.000000000000000000, 1.000000000000000000, 1.000000000000000000, 1.000000000000000000, 1.000000000000000000, 1.000000000000000000, 1.000000000000000000, 1.000000000000000000, 1.000000000000000000, 1.000000000000000000, 1.000000000000000000, 1.000000000000000000, 1.000000000000000000, 1.000000000000000000, 1.000000000000000000, 1.000000000000000000, 1.000000000000000000, 1.000000000000000000, 1.000000000000000000, 1.000000000000000000, 1.000000000000000000, 1.000000000000000000, 1.000000000000000000, 1.000000000000000000, 1.000000000000000000, 1.000000000000000000, 1.000000000000000000, 1.000000000000000000, 1.000000000000000000, 1.000000000000000000, 1.000000000000000000, 1.000000000000000000, 1.000000000000000000, 1.000000000000000000, 1.000000000000000000, 1.000000000000000000, 1.000000000000000000, 1.000000000000000000, 1.000000000000000000, 1.000000000000000000, 1.000000000000000000),
 ( 0.3333333333333333703, 0.3333333333333333703, 0.3333333333333333703, 0.3333333333333333703, 0.3333333333333333703, 0.3333333333333333703, 0.3333333333333333703, 0.3333333333333333703, 0.3333333333333333703, 0.3333333333333333703, 0.3333333333333333703, 0.3333333333333333703, 0.3333333333333333703, 0.3333333333333333703, 0.3333333333333333703, 0.3333333333333333703, 0.3333333333333333703, 0.3333333333333333703, 0.3333333333333333703, 0.3333333333333333703, 0.3333333333333333703, 0.3333333333333333703, 0.3333333333333333703, 0.3333333333333333703, 0.3333333333333333703, 0.3333333333333333703, 0.3333333333333333703, 0.3333333333333333703, 0.3333333333333333703, 0.3333333333333333703, 0.3333333333333333703, 0.3333333333333333703, 0.3333333333333333703, 0.3333333333333333703, 0.3333333333333333703, 0.3333333333333333703, 0.3333333333333333703, 0.3333333333333333703, 0.3333333333333333703, 0.3333333333333333703, 0.3333333333333333703, 0.3333333333333333703, 0.3333333333333333703, 0.3333333333333333703, 0.3333333333333333703, 0.3333333333333333703, 0.3333333333333333703, 0.3333333333333333703, 0.3333333333333333703, 0.3333333333333333703, 0.3333333333333333703, 0.3333333333333333703, 0.3333333333333333703, 0.3333333333333333703, 0.3333333333333333703, 0.3333333333333333703, 0.3333333333333333703, 0.3333333333333333703, 0.3333333333333333703, 0.3333333333333333703, 0.3333333333333333703, 0.3333333333333333703, 0.3333333333333333703, 0.3333333333333333703, 0.3333333333333333703, 0.3333333333333333703, 0.3333333333333333703, 0.3333333333333333703, 0.3333333333333333703, 0.3333333333333333703, 0.3333333333333333703, 0.3333333333333333703, 0.3333333333333333703, 0.3333333333333333703, 0.3333333333333333703, 0.3333333333333333703, 0.3333333333333333703, 0.3333333333333333703, 0.3333333333333333703, 0.3333333333333333703, 0.3333333333333333703, 0.3333333333333333703, 0.3333333333333333703, 0.3333333333333333703, 0.3333333333333333703, 0.3333333333333333703, 0.3333333333333333703, 0.3333333333333333703, 0.3333333333333333703, 0.3333333333333333703, 0.3333333333333333703, 0.3333333333333333703, 0.3333333333333333703, 0.3333333333333333703, 0.3333333333333333703, 0.3333333333333333703, 0.3333333333333333703, 0.3333333333333333703, 0.3333333333333333703, 0.3333333333333333703, 0.3333333333333333703, 0.3333333333333333703, 0.3333333333333333703, 0.3333333333333333703, 0.3333333333333333703, 0.3333333333333333703, 0.3333333333333333703, 0.3333333333333333703, 0.3333333333333333703, 0.3333333333333333703, 0.3333333333333333703, 0.3333333333333333703, 0.3333333333333333703, 0.3333333333333333703, 0.3333333333333333703, 0.3333333333333333703, 0.3333333333333333703, 0.3333333333333333703, 0.3333333333333333703, 0.3333333333333333703, 0.3333333333333333703, 0.3333333333333333703, 0.3333333333333333703, 0.3333333333333333703, 0.3333333333333333703, 0.3333333333333333703, 0.3333333333333333703, 0.3333333333333333703, 0.3333333333333333703, 0.3333333333333333703, 0.3333333333333333703, 0.3333333333333333703, 0.3333333333333333703, 0.3333333333333333703, 0.3333333333333333703, 0.3333333333333333703, 0.3333333333333333703, 0.3333333333333333703, 0.3333333333333333703, 0.3333333333333333703, 0.3333333333333333703, 0.3333333333333333703, 0.3333333333333333703, 0.3333333333333333703, 0.3333333333333333703, 0.3333333333333333703, 0.3333333333333333703, 0.3333333333333333703, 0.3333333333333333703, 0.3333333333333333703, 0.3333333333333333703, 0.3333333333333333703, 0.3333333333333333703, 0.3333333333333333703, 0.3333333333333333703, 0.3333333333333333703, 0.3333333333333333703, 0.3333333333333333703, 0.3333333333333333703, 0.3333333333333333703, 0.3333333333333333703, 0.3333333333333333703, 0.3333333333333333703, 0.3333333333333333703, 0.3333333333333333703, 0.3333333333333333703, 0.3333333333333333703, 0.3333333333333333703, 0.3333333333333333703, 0.3333333333333333703, 0.3333333333333333703, 0.3333333333333333703, 0.3333333333333333703, 0.3333333333333333703, 0.3333333333333333703, 0.3333333333333333703, 0.3333333333333333703, 0.3333333333333333703, 0.3333333333333333703, 0.3333333333333333703, 0.3333333333333333703, 0.3333333333333333703, 0.3333333333333333703, 0.3333333333333333703, 0.3333333333333333703, 0.3333333333333333703, 0.3333333333333333703, 0.3333333333333333703, 0.3333333333333333703, 0.3333333333333333703, 0.3333333333333333703, 0.3333333333333333703, 0.3333333333333333703, 0.3333333333333333703, 0.3333333333333333703, 0.3333333333333333703, 0.3333333333333333703, 0.3333333333333333703, 0.3333333333333333703, 0.3333333333333333703, 0.3333333333333333703, 0.3333333333333333703, 0.3333333333333333703, 0.3333333333333333703, 0.3333333333333333703, 0.3333333333333333703, 0.3333333333333333703, 0.3333333333333333703, 0.3333333333333333703, 0.3333333333333333703, 0.3333333333333333703, 0.3333333333333333703, 0.3333333333333333703, 0.3333333333333333703, 0.3333333333333333703, 0.3333333333333333703, 0.3333333333333333703, 0.3333333333333333703, 0.3333333333333333703, 0.3333333333333333703, 0.3333333333333333703, 0.3333333333333333703, 0.3333333333333333703, 0.3333333333333333703, 0.3333333333333333703, 0.3333333333333333703, 0.3333333333333333703, 0.3333333333333333703, 0.3333333333333333703, 0.3333333333333333703, 0.3333333333333333703, 0.3333333333333333703, 0.3333333333333333703, 0.3333333333333333703, 0.3333333333333333703, 0.3333333333333333703, 0.3333333333333333703, 0.3333333333333333703, 0.3333333333333333703, 0.3333333333333333703, 0.3333333333333333703, 0.3333333333333333703, 0.3333333333333333703, 0.3333333333333333703, 0.3333333333333333703, 0.3333333333333333703, 0.3333333333333333703, 0.3333333333333333703, 0.3333333333333333703, 0.3333333333333333703, 0.3333333333333333703, 0.3333333333333333703, 0.3333333333333333703, 0.3333333333333333703, 0.3333333333333333703, 0.3333333333333333703, 0.3333333333333333703, 0.3333333333333333703, 0.3333333333333333703, 0.3333333333333333703, 0.3333333333333333703, 0.3333333333333333703, 0.3333333333333333703, 0.3333333333333333703, 0.3333333333333333703, 0.3333333333333333703, 0.3333333333333333703, 0.3333333333333333703, 0.3333333333333333703, 0.3333333333333333703, 0.3333333333333333703, 0.3333333333333333703, 0.3333333333333333703, 0.3333333333333333703, 0.3333333333333333703, 0.3333333333333333703, 0.3333333333333333703, 0.3333333333333333703, 0.3333333333333333703, 0.3333333333333333703, 0.3333333333333333703, 0.3333333333333333703, 0.3333333333333333703, 0.3333333333333333703, 0.3333333333333333703, 0.3333333333333333703, 0.3333333333333333703, 0.3333333333333333703, 0.3333333333333333703, 0.3333333333333333703, 0.3333333333333333703, 0.3333333333333333703, 0.3333333333333333703, 0.3333333333333333703, 0.3333333333333333703, 0.3333333333333333703, 0.3333333333333333703, 0.3333333333333333703, 0.3333333333333333703, 0.3333333333333333703, 0.3333333333333333703, 0.3333333333333333703, 0.3333333333333333703, 0.3333333333333333703, 0.3333333333333333703, 0.3333333333333333703, 0.3333333333333333703, 0.3333333333333333703, 0.3333333333333333703, 0.3333333333333333703, 0.3333333333333333703, 0.3333333333333333703, 0.3333333333333333703, 0.3333333333333333703, 0.3333333333333333703, 0.3333333333333333703, 0.3333333333333333703, 0.3333333333333333703, 0.3333333333333333703, 0.3333333333333333703, 0.3333333333333333703, 0.3333333333333333703, 0.3333333333333333703, 0.3333333333333333703, 0.3333333333333333703, 0.3333333333333333703, 0.3333333333333333703, 0.3333333333333333703, 0.3333333333333333703, 0.3333333333333333703, 0.3333333333333333703, 0.3333333333333333703, 0.3333333333333333703, 0.3333333333333333703, 0.3333333333333333703, 0.3333333333333333703),
 ( 0.3333333333333333703, 0.3333333333333333703, 0.3333333333333333703, 0.3333333333333333703, 0.3333333333333333703, 0.3333333333333333703, 0.3333333333333333703, 0.3333333333333333703, 0.3333333333333333703, 0.3333333333333333703, 0.3333333333333333703, 0.3333333333333333703, 0.3333333333333333703, 0.3333333333333333703, 0.3333333333333333703, 0.3333333333333333703, 0.3333333333333333703, 0.3333333333333333703, 0.3333333333333333703, 0.3333333333333333703, 0.3333333333333333703, 0.3333333333333333703, 0.3333333333333333703, 0.3333333333333333703, 0.3333333333333333703, 0.3333333333333333703, 0.3333333333333333703, 0.3333333333333333703, 0.3333333333333333703, 0.3333333333333333703, 0.3333333333333333703, 0.3333333333333333703, 0.3333333333333333703, 0.3333333333333333703, 0.3333333333333333703, 0.3333333333333333703, 0.3333333333333333703, 0.3333333333333333703, 0.3333333333333333703, 0.3333333333333333703, 0.3333333333333333703, 0.3333333333333333703, 0.3333333333333333703, 0.3333333333333333703, 0.3333333333333333703, 0.3333333333333333703, 0.3333333333333333703, 0.3333333333333333703, 0.3333333333333333703, 0.3333333333333333703, 0.3333333333333333703, 0.3333333333333333703, 0.3333333333333333703, 0.3333333333333333703, 0.3333333333333333703, 0.3333333333333333703, 0.3333333333333333703, 0.3333333333333333703, 0.3333333333333333703, 0.3333333333333333703, 0.3333333333333333703, 0.3333333333333333703, 0.3333333333333333703, 0.3333333333333333703, 0.3333333333333333703, 0.3333333333333333703, 0.3333333333333333703, 0.3333333333333333703, 0.3333333333333333703, 0.3333333333333333703, 0.3333333333333333703, 0.3333333333333333703, 0.3333333333333333703, 0.3333333333333333703, 0.3333333333333333703, 0.3333333333333333703, 0.3333333333333333703, 0.3333333333333333703, 0.3333333333333333703, 0.3333333333333333703, 0.3333333333333333703, 0.3333333333333333703, 0.3333333333333333703, 0.3333333333333333703, 0.3333333333333333703, 0.3333333333333333703, 0.3333333333333333703, 0.3333333333333333703, 0.3333333333333333703, 0.3333333333333333703, 0.3333333333333333703, 0.3333333333333333703, 0.3333333333333333703, 0.3333333333333333703, 0.3333333333333333703, 0.3333333333333333703, 0.3333333333333333703, 0.3333333333333333703, 0.3333333333333333703, 0.3333333333333333703, 0.3333333333333333703, 0.3333333333333333703, 0.3333333333333333703, 0.3333333333333333703, 0.3333333333333333703, 0.3333333333333333703, 0.3333333333333333703, 0.3333333333333333703, 0.3333333333333333703, 0.3333333333333333703, 0.3333333333333333703, 0.3333333333333333703, 0.3333333333333333703, 0.3333333333333333703, 0.3333333333333333703, 0.3333333333333333703, 0.3333333333333333703, 0.3333333333333333703, 0.3333333333333333703, 0.3333333333333333703, 0.3333333333333333703, 0.3333333333333333703, 0.3333333333333333703, 0.3333333333333333703, 0.3333333333333333703, 0.3333333333333333703, 0.3333333333333333703, 0.3333333333333333703, 0.3333333333333333703, 0.3333333333333333703, 0.3333333333333333703, 0.3333333333333333703, 0.3333333333333333703, 0.3333333333333333703, 0.3333333333333333703, 0.3333333333333333703, 0.3333333333333333703, 0.3333333333333333703, 0.3333333333333333703, 0.3333333333333333703, 0.3333333333333333703, 0.3333333333333333703, 0.3333333333333333703, 0.3333333333333333703, 0.3333333333333333703, 0.3333333333333333703, 0.3333333333333333703, 0.3333333333333333703, 0.3333333333333333703, 0.3333333333333333703, 0.3333333333333333703, 0.3333333333333333703, 0.3333333333333333703, 0.3333333333333333703, 0.3333333333333333703, 0.3333333333333333703, 0.3333333333333333703, 0.3333333333333333703, 0.3333333333333333703, 0.3333333333333333703, 0.3333333333333333703, 0.3333333333333333703, 0.3333333333333333703, 0.3333333333333333703, 0.3333333333333333703, 0.3333333333333333703, 0.3333333333333333703, 0.3333333333333333703, 0.3333333333333333703, 0.3333333333333333703, 0.3333333333333333703, 0.3333333333333333703, 0.3333333333333333703, 0.3333333333333333703, 0.3333333333333333703, 0.3333333333333333703, 0.3333333333333333703, 0.3333333333333333703, 0.3333333333333333703, 0.3333333333333333703, 0.3333333333333333703, 0.3333333333333333703, 0.3333333333333333703, 0.3333333333333333703, 0.3333333333333333703, 0.3333333333333333703, 0.3333333333333333703, 0.3333333333333333703, 0.3333333333333333703, 0.3333333333333333703, 0.3333333333333333703, 0.3333333333333333703, 0.3333333333333333703, 0.3333333333333333703, 0.3333333333333333703, 0.3333333333333333703, 0.3333333333333333703, 0.3333333333333333703, 0.3333333333333333703, 0.3333333333333333703, 0.3333333333333333703, 0.3333333333333333703, 0.3333333333333333703, 0.3333333333333333703, 0.3333333333333333703, 0.3333333333333333703, 0.3333333333333333703, 0.3333333333333333703, 0.3333333333333333703, 0.3333333333333333703, 0.3333333333333333703, 0.3333333333333333703, 0.3333333333333333703, 0.3333333333333333703, 0.3333333333333333703, 0.3333333333333333703, 0.3333333333333333703, 0.3333333333333333703, 0.3333333333333333703, 0.3333333333333333703, 0.3333333333333333703, 0.3333333333333333703, 0.3333333333333333703, 0.3333333333333333703, 0.3333333333333333703, 0.3333333333333333703, 0.3333333333333333703, 0.3333333333333333703, 0.3333333333333333703, 0.3333333333333333703, 0.3333333333333333703, 0.3333333333333333703, 0.3333333333333333703, 0.3333333333333333703, 0.3333333333333333703, 0.3333333333333333703, 0.3333333333333333703, 0.3333333333333333703, 0.3333333333333333703, 0.3333333333333333703, 0.3333333333333333703, 0.3333333333333333703, 0.3333333333333333703, 0.3333333333333333703, 0.3333333333333333703, 0.3333333333333333703, 0.3333333333333333703, 0.3333333333333333703, 0.3333333333333333703, 0.3333333333333333703, 0.3333333333333333703, 0.3333333333333333703, 0.3333333333333333703, 0.3333333333333333703, 0.3333333333333333703, 0.3333333333333333703, 0.3333333333333333703, 0.3333333333333333703, 0.3333333333333333703, 0.3333333333333333703, 0.3333333333333333703, 0.3333333333333333703, 0.3333333333333333703, 0.3333333333333333703, 0.3333333333333333703, 0.3333333333333333703, 0.3333333333333333703, 0.3333333333333333703, 0.3333333333333333703, 0.3333333333333333703, 0.3333333333333333703, 0.3333333333333333703, 0.3333333333333333703, 0.3333333333333333703, 0.3333333333333333703, 0.3333333333333333703, 0.3333333333333333703, 0.3333333333333333703, 0.3333333333333333703, 0.3333333333333333703, 0.3333333333333333703, 0.3333333333333333703, 0.3333333333333333703, 0.3333333333333333703, 0.3333333333333333703, 0.3333333333333333703, 0.3333333333333333703, 0.3333333333333333703, 0.3333333333333333703, 0.3333333333333333703, 0.3333333333333333703, 0.3333333333333333703, 0.3333333333333333703, 0.3333333333333333703, 0.3333333333333333703, 0.3333333333333333703, 0.3333333333333333703, 0.3333333333333333703, 0.3333333333333333703, 0.3333333333333333703, 0.3333333333333333703, 0.3333333333333333703, 0.3333333333333333703, 0.3333333333333333703, 0.3333333333333333703, 0.3333333333333333703, 0.3333333333333333703, 0.3333333333333333703, 0.3333333333333333703, 0.3333333333333333703, 0.3333333333333333703, 0.3333333333333333703, 0.3333333333333333703, 0.3333333333333333703, 0.3333333333333333703, 0.3333333333333333703, 0.3333333333333333703, 0.3333333333333333703, 0.3333333333333333703, 0.3333333333333333703, 0.3333333333333333703, 0.3333333333333333703, 0.3333333333333333703, 0.3333333333333333703, 0.3333333333333333703, 0.3333333333333333703, 0.3333333333333333703, 0.3333333333333333703, 0.3333333333333333703, 0.3333333333333333703, 0.3333333333333333703, 0.3333333333333333703, 0.3333333333333333703, 0.3333333333333333703, 0.3333333333333333703, 0.3333333333333333703),
 ( 1.000000000000000000, 1.000000000000000000, 1.000000000000000000, 1.000000000000000000, 1.000000000000000000, 1.000000000000000000, 1.000000000000000000, 1.000000000000000000, 1.000000000000000000, 1.000000000000000000, 1.000000000000000000, 1.000000000000000000, 1.000000000000000000, 1.000000000000000000, 1.000000000000000000, 1.000000000000000000, 1.000000000000000000, 1.000000000000000000, 1.000000000000000000, 1.000000000000000000, 1.000000000000000000, 1.000000000000000000, 1.000000000000000000, 1.000000000000000000, 1.000000000000000000, 1.000000000000000000, 1.000000000000000000, 1.000000000000000000, 1.000000000000000000, 1.000000000000000000, 1.000000000000000000, 1.000000000000000000, 1.000000000000000000, 1.000000000000000000, 1.000000000000000000, 1.000000000000000000, 1.000000000000000000, 1.000000000000000000, 1.000000000000000000, 1.000000000000000000, 1.000000000000000000, 1.000000000000000000, 1.000000000000000000, 1.000000000000000000, 1.000000000000000000, 1.000000000000000000, 1.000000000000000000, 1.000000000000000000, 1.000000000000000000, 1.000000000000000000, 1.000000000000000000, 1.000000000000000000, 1.000000000000000000, 1.000000000000000000, 1.000000000000000000, 1.000000000000000000, 1.000000000000000000, 1.000000000000000000, 1.000000000000000000, 1.000000000000000000, 1.000000000000000000, 1.000000000000000000, 1.000000000000000000, 1.000000000000000000, 1.000000000000000000, 1.000000000000000000, 1.000000000000000000, 1.000000000000000000, 1.000000000000000000, 1.000000000000000000, 1.000000000000000000, 1.000000000000000000, 1.000000000000000000, 1.000000000000000000, 1.000000000000000000, 1.000000000000000000, 1.000000000000000000, 1.000000000000000000, 1.000000000000000000, 1.000000000000000000, 1.000000000000000000, 1.000000000000000000, 1.000000000000000000, 1.000000000000000000, 1.000000000000000000, 1.000000000000000000, 1.000000000000000000, 1.000000000000000000, 1.000000000000000000, 1.000000000000000000, 1.000000000000000000, 1.000000000000000000, 1.000000000000000000, 1.000000000000000000, 1.000000000000000000, 1.000000000000000000, 1.000000000000000000, 1.000000000000000000, 1.000000000000000000, 1.000000000000000000, 1.000000000000000000, 1.000000000000000000, 1.000000000000000000, 1.000000000000000000, 1.000000000000000000, 1.000000000000000000, 1.000000000000000000, 1.000000000000000000, 1.000000000000000000, 1.000000000000000000, 1.000000000000000000, 1.000000000000000000, 1.000000000000000000, 1.000000000000000000, 1.000000000000000000, 1.000000000000000000, 1.000000000000000000, 1.000000000000000000, 1.000000000000000000, 1.000000000000000000, 1.000000000000000000, 1.000000000000000000, 1.000000000000000000, 1.000000000000000000, 1.000000000000000000, 1.000000000000000000, 1.000000000000000000, 1.000000000000000000, 1.000000000000000000, 1.000000000000000000, 1.000000000000000000, 1.000000000000000000, 1.000000000000000000, 1.000000000000000000, 1.000000000000000000, 1.000000000000000000, 1.000000000000000000, 1.000000000000000000, 1.000000000000000000, 1.000000000000000000, 1.000000000000000000, 1.000000000000000000, 1.000000000000000000, 1.000000000000000000, 1.000000000000000000, 1.000000000000000000, 1.000000000000000000, 1.000000000000000000, 1.000000000000000000, 1.000000000000000000, 1.000000000000000000, 1.000000000000000000, 1.000000000000000000, 1.000000000000000000, 1.000000000000000000, 1.000000000000000000, 1.000000000000000000, 1.000000000000000000, 1.000000000000000000, 1.000000000000000000, 1.000000000000000000, 1.000000000000000000, 1.000000000000000000, 1.000000000000000000, 1.000000000000000000, 1.000000000000000000, 1.000000000000000000, 1.000000000000000000, 1.000000000000000000, 1.000000000000000000, 1.000000000000000000, 1.000000000000000000, 1.000000000000000000, 1.000000000000000000, 1.000000000000000000, 1.000000000000000000, 1.000000000000000000, 1.000000000000000000, 1.000000000000000000, 1.000000000000000000, 1.000000000000000000, 1.000000000000000000, 1.000000000000000000, 1.000000000000000000, 1.000000000000000000, 1.000000000000000000, 1.000000000000000000, 1.000000000000000000, 1.000000000000000000, 1.000000000000000000, 1.000000000000000000, 1.000000000000000000, 1.000000000000000000, 1.000000000000000000, 1.000000000000000000, 1.000000000000000000, 1.000000000000000000, 1.000000000000000000, 1.000000000000000000, 1.000000000000000000, 1.000000000000000000, 1.000000000000000000, 1.000000000000000000, 1.000000000000000000, 1.000000000000000000, 1.000000000000000000, 1.000000000000000000, 1.000000000000000000, 1.000000000000000000, 1.000000000000000000, 1.000000000000000000, 1.000000000000000000, 1.000000000000000000, 1.000000000000000000, 1.000000000000000000, 1.000000000000000000, 1.000000000000000000, 1.000000000000000000, 1.000000000000000000, 1.000000000000000000, 1.000000000000000000, 1.000000000000000000, 1.000000000000000000, 1.000000000000000000, 1.000000000000000000, 1.000000000000000000, 1.000000000000000000, 1.000000000000000000, 1.000000000000000000, 1.000000000000000000, 1.000000000000000000, 1.000000000000000000, 1.000000000000000000, 1.000000000000000000, 1.000000000000000000, 1.000000000000000000, 1.000000000000000000, 1.000000000000000000, 1.000000000000000000, 1.000000000000000000, 1.000000000000000000, 1.000000000000000000, 1.000000000000000000, 1.000000000000000000, 1.000000000000000000, 1.000000000000000000, 1.000000000000000000, 1.000000000000000000, 1.000000000000000000, 1.000000000000000000, 1.000000000000000000, 1.000000000000000000, 1.000000000000000000, 1.000000000000000000, 1.000000000000000000, 1.000000000000000000, 1.000000000000000000, 1.000000000000000000, 1.000000000000000000, 1.000000000000000000, 1.000000000000000000, 1.000000000000000000, 1.000000000000000000, 1.000000000000000000, 1.000000000000000000, 1.000000000000000000, 1.000000000000000000, 1.000000000000000000, 1.000000000000000000, 1.000000000000000000, 1.000000000000000000, 1.000000000000000000, 1.000000000000000000, 1.000000000000000000, 1.000000000000000000, 1.000000000000000000, 1.000000000000000000, 1.000000000000000000, 1.000000000000000000, 1.000000000000000000, 1.000000000000000000, 1.000000000000000000, 1.000000000000000000, 1.000000000000000000, 1.000000000000000000, 1.000000000000000000, 1.000000000000000000, 1.000000000000000000, 1.000000000000000000, 1.000000000000000000, 1.000000000000000000, 1.000000000000000000, 1.000000000000000000, 1.000000000000000000, 1.000000000000000000, 1.000000000000000000, 1.000000000000000000, 1.000000000000000000, 1.000000000000000000, 1.000000000000000000, 1.000000000000000000, 1.000000000000000000, 1.000000000000000000, 1.000000000000000000, 1.000000000000000000, 1.000000000000000000, 1.000000000000000000, 1.000000000000000000, 1.000000000000000000, 1.000000000000000000, 1.000000000000000000, 1.000000000000000000, 1.000000000000000000, 1.000000000000000000, 1.000000000000000000, 1.000000000000000000, 1.000000000000000000, 1.000000000000000000, 1.000000000000000000, 1.000000000000000000, 1.000000000000000000, 1.000000000000000000, 1.000000000000000000, 1.000000000000000000, 1.000000000000000000, 1.000000000000000000, 1.000000000000000000, 1.000000000000000000, 1.000000000000000000, 1.000000000000000000, 1.000000000000000000, 1.000000000000000000, 1.000000000000000000, 1.000000000000000000, 1.000000000000000000, 1.000000000000000000) ) ) 
 REPRESENTATION_ITEM ( '' )  SURFACE ( )  );
#3700 = AXIS2_PLACEMENT_3D ( 'NONE', #20546, #10329, #10549 ) ;
#3701 = CARTESIAN_POINT ( 'NONE',  ( -27.92885697401080591, 6.962042978589167319, -220.9552227796709190 ) ) ;
#3702 = CARTESIAN_POINT ( 'NONE',  ( 6.566035546683759883, 15.06745272174450712, -218.8330720708048034 ) ) ;
#3703 = CARTESIAN_POINT ( 'NONE',  ( -2.129100187576105530, 26.11057959790866789, -231.5939360033278547 ) ) ;
#3704 = ORIENTED_EDGE ( 'NONE', *, *, #11353, .F. ) ;
#3705 = CARTESIAN_POINT ( 'NONE',  ( 23.82514222742702614, -14.35463969081363267, -233.5616060903067535 ) ) ;
#3706 = ORIENTED_EDGE ( 'NONE', *, *, #17805, .T. ) ;
#3707 = CARTESIAN_POINT ( 'NONE',  ( 13.43730899468209294, 8.427513769504761498, -221.4030804848920297 ) ) ;
#3708 = CARTESIAN_POINT ( 'NONE',  ( -8.005900519654911562, 11.01772743098285545, -228.7074549843708269 ) ) ;
#3709 = CARTESIAN_POINT ( 'NONE',  ( -20.95553895916151177, 12.88782924195037438, -232.2493899712447956 ) ) ;
#3710 = CARTESIAN_POINT ( 'NONE',  ( -8.326748185965973548, -13.59788789161040512, -220.4531618457016862 ) ) ;
#3711 = CARTESIAN_POINT ( 'NONE',  ( -20.54164754914381064, 7.122791156791981493, -233.5720402887671980 ) ) ;
#3712 = DIRECTION ( 'NONE',  ( -0.000000000000000000, 0.000000000000000000, -1.000000000000000000 ) ) ;
#3713 = FACE_OUTER_BOUND ( 'NONE', #10038, .T. ) ;
#3714 = LINE ( 'NONE', #4051, #14959 ) ;
#3715 = VECTOR ( 'NONE', #6158, 1000.000000000000000 ) ;
#3716 = CARTESIAN_POINT ( 'NONE',  ( -11.55316006017064012, 19.79513644261079719, -232.3088878043970453 ) ) ;
#3717 = CARTESIAN_POINT ( 'NONE',  ( 15.65443801613259467, 7.488839228060037989, -233.6469817377710569 ) ) ;
#3718 = CARTESIAN_POINT ( 'NONE',  ( -20.94800339253696109, 4.477632454355491731, -216.5423208360950298 ) ) ;
#3719 = EDGE_CURVE ( 'NONE', #16840, #4321, #11664, .T. ) ;
#3720 = CARTESIAN_POINT ( 'NONE',  ( -16.01199461824852932, -9.140529685459805265, -215.3147469429904106 ) ) ;
#3721 = CARTESIAN_POINT ( 'NONE',  ( -20.63475909113443763, -3.483688486440585486, -233.7225001494461480 ) ) ;
#3722 = CARTESIAN_POINT ( 'NONE',  ( -7.694246740028670928, 10.31295298368923063, -221.9989544301487001 ) ) ;
#3723 = CARTESIAN_POINT ( 'NONE',  ( -12.42894476027428929, -17.97759322220185396, -216.3110355466728834 ) ) ;
#3724 = CARTESIAN_POINT ( 'NONE',  ( 15.12287735332712835, 21.03907941686458116, -231.7894952627153202 ) ) ;
#3725 = CARTESIAN_POINT ( 'NONE',  ( 15.44393261315032184, -28.37553556939610999, -226.2064134899511600 ) ) ;
#3726 = DIRECTION ( 'NONE',  ( -1.000000000000000000, 0.000000000000000000, 0.000000000000000000 ) ) ;
#3727 = CARTESIAN_POINT ( 'NONE',  ( 21.27683256847563698, 4.223177115764435108, -215.2584548172064842 ) ) ;
#3728 = CARTESIAN_POINT ( 'NONE',  ( 0.000000000000000000, 22.63401512838748175, 77.51594804401857175 ) ) ;
#3729 = CARTESIAN_POINT ( 'NONE',  ( 0.6289891638115701067, 16.47510600144228832, -227.0521699048171342 ) ) ;
#3730 = CARTESIAN_POINT ( 'NONE',  ( -29.22672729369577738, 6.588740615114764054, -224.9915299386302934 ) ) ;
#3731 = CARTESIAN_POINT ( 'NONE',  ( 24.03642272140365677, 3.646960756862087205, -218.2320643939070806 ) ) ;
#3732 = CARTESIAN_POINT ( 'NONE',  ( 24.52160379727246209, 5.049198597839295033, -215.7868787176665535 ) ) ;
#3733 = CARTESIAN_POINT ( 'NONE',  ( 1.040523496405688642, -16.53460264249922318, -217.0944950338946455 ) ) ;
#3734 = CARTESIAN_POINT ( 'NONE',  ( 2.469769522101480597, 18.85781121334172639, -215.5372409425634430 ) ) ;
#3735 = AXIS2_PLACEMENT_3D ( 'NONE', #3451, #6496, #8200 ) ;
#3736 = CARTESIAN_POINT ( 'NONE',  ( -3.350277215847999202, -25.10023987965119119, -233.9767109426786647 ) ) ;
#3737 = CARTESIAN_POINT ( 'NONE',  ( -16.50467377682197423, 21.56569464670658220, -229.9175202103629374 ) ) ;
#3738 = CARTESIAN_POINT ( 'NONE',  ( 23.18902850759750933, 20.27908137164207147, -226.2847847834817117 ) ) ;
#3739 = CARTESIAN_POINT ( 'NONE',  ( -28.87859926594958537, -0.8320174534291842061, -222.6356913548140142 ) ) ;
#3740 = CARTESIAN_POINT ( 'NONE',  ( -22.03660207690921879, 17.07234836129451949, -222.7335359861421296 ) ) ;
#3741 = CARTESIAN_POINT ( 'NONE',  ( -0.2758005215353623862, 11.79991891162212525, -226.8645588387054488 ) ) ;
#3742 = CARTESIAN_POINT ( 'NONE',  ( 15.70515172005171323, -0.7403987186381333352, -226.4590404369862995 ) ) ;
#3743 = ORIENTED_EDGE ( 'NONE', *, *, #15073, .F. ) ;
#3744 = EDGE_CURVE ( 'NONE', #17843, #1266, #319, .T. ) ;
#3745 = CARTESIAN_POINT ( 'NONE',  ( 16.26678737605450564, -16.61684638199339048, -230.8698708339908308 ) ) ;
#3746 = VERTEX_POINT ( 'NONE', #18649 ) ;
#3747 = CARTESIAN_POINT ( 'NONE',  ( 14.68951511424354273, -18.85605729411972575, -217.5026406474102885 ) ) ;
#3748 = CARTESIAN_POINT ( 'NONE',  ( -8.752190949579933488, 24.25633523490762755, -230.6624101830059885 ) ) ;
#3749 = ORIENTED_EDGE ( 'NONE', *, *, #4848, .T. ) ;
#3750 = TOROIDAL_SURFACE ( 'NONE', #8452, 22.00000000000000711, 2.999999999999999112 ) ;
#3751 = CARTESIAN_POINT ( 'NONE',  ( 12.53674998645855787, 17.96979015029927851, -232.8843215672231679 ) ) ;
#3752 = CARTESIAN_POINT ( 'NONE',  ( -23.51371042417668633, 2.081716773471995463, -216.9231029201042418 ) ) ;
#3753 = CARTESIAN_POINT ( 'NONE',  ( -18.64257584594551531, -16.66392856591270899, -217.1407738418131999 ) ) ;
#3754 = CARTESIAN_POINT ( 'NONE',  ( -1.542335193334551491, -19.71915426430242135, -216.1352730594569209 ) ) ;
#3755 = CARTESIAN_POINT ( 'NONE',  ( -6.573387563318148885, 17.69612765735440973, -231.1211991061559274 ) ) ;
#3756 = DIRECTION ( 'NONE',  ( 0.000000000000000000, 1.000000000000000000, -1.224646799147353207E-16 ) ) ;
#3757 = CARTESIAN_POINT ( 'NONE',  ( 18.90025403853754327, 17.70150481658638952, -229.5234643039372315 ) ) ;
#3758 = CARTESIAN_POINT ( 'NONE',  ( -8.823862513872974489, 14.92351368520778898, -217.1499513473673346 ) ) ;
#3759 = CARTESIAN_POINT ( 'NONE',  ( -5.706122936196527107, 15.14201253431006045, -228.6865785740211550 ) ) ;
#3760 = VERTEX_POINT ( 'NONE', #3210 ) ;
#3761 = CARTESIAN_POINT ( 'NONE',  ( 2.535512286608554433, 13.86868953312499109, -224.9313928733152181 ) ) ;
#3762 = CARTESIAN_POINT ( 'NONE',  ( -17.64438593497130370, 2.824953307685432069, -229.4443205246391813 ) ) ;
#3763 = CARTESIAN_POINT ( 'NONE',  ( 22.69522586737246783, 3.669837464059151344, -234.0947686933411944 ) ) ;
#3764 = EDGE_CURVE ( 'NONE', #18119, #1644, #21848, .T. ) ;
#3765 = CARTESIAN_POINT ( 'NONE',  ( 8.211296573249146746, -12.45047565346596130, -222.1279395315445413 ) ) ;
#3766 = LINE ( 'NONE', #5233, #14334 ) ;
#3767 = CARTESIAN_POINT ( 'NONE',  ( -22.00000000000137490, -2.602085213965210642E-15, -216.9999999999999716 ) ) ;
#3768 = CARTESIAN_POINT ( 'NONE',  ( -3.501680520304516264, 14.31538576447642264, -219.8967178229432307 ) ) ;
#3769 = CARTESIAN_POINT ( 'NONE',  ( 15.75976565806011465, -3.644771625422815298, -224.1463364774561740 ) ) ;
#3770 = CARTESIAN_POINT ( 'NONE',  ( 29.17814965709308694, -1.309718763918959139, -225.2029557489520926 ) ) ;
#3771 = CARTESIAN_POINT ( 'NONE',  ( 13.69275646168278371, 8.674223198772375909, -220.8699857572541987 ) ) ;
#3772 = ADVANCED_FACE ( 'NONE', ( #20650 ), #19189, .T. ) ;
#3773 = CARTESIAN_POINT ( 'NONE',  ( -17.96792326766206926, -0.6237852504629022299, -217.9759415197746932 ) ) ;
#3774 = AXIS2_PLACEMENT_3D ( 'NONE', #4834, #4714, #16779 ) ;
#3775 = VECTOR ( 'NONE', #17147, 1000.000000000000000 ) ;
#3776 = CARTESIAN_POINT ( 'NONE',  ( 2.178520447619924472, -13.56847537563065487, -221.4085897031499428 ) ) ;
#3777 = CARTESIAN_POINT ( 'NONE',  ( 0.000000000000000000, 0.000000000000000000, 0.000000000000000000 ) ) ;
#3778 = CARTESIAN_POINT ( 'NONE',  ( -11.98736441306973077, 11.45674391201457176, -217.8252237716743025 ) ) ;
#3779 = CARTESIAN_POINT ( 'NONE',  ( -8.929606928624414408, 11.65278034267609186, -219.1999234847403386 ) ) ;
#3780 = ORIENTED_EDGE ( 'NONE', *, *, #989, .F. ) ;
#3781 = CARTESIAN_POINT ( 'NONE',  ( -24.48580119005125866, 9.312492396273500006, -232.5498413856076070 ) ) ;
#3782 = CARTESIAN_POINT ( 'NONE',  ( -19.98462433625633494, -12.30084073857678639, -216.8518508258974862 ) ) ;
#3783 = CARTESIAN_POINT ( 'NONE',  ( 0.000000000000000000, -23.00000000000006040, -30.00000000000000000 ) ) ;
#3784 = CARTESIAN_POINT ( 'NONE',  ( 0.000000000000000000, 0.000000000000000000, -77.51594804401857175 ) ) ;
#3785 = CARTESIAN_POINT ( 'NONE',  ( -23.98802705797876200, 19.46654170242919690, -223.5293093576406989 ) ) ;
#3786 = CARTESIAN_POINT ( 'NONE',  ( 0.3570725323625942860, -15.31465789365257102, -218.3993834748477525 ) ) ;
#3787 = FILL_AREA_STYLE_COLOUR ( '', #4518 ) ;
#3788 = CARTESIAN_POINT ( 'NONE',  ( 18.83061188870375702, -2.941116900365129183, -225.6031553348211958 ) ) ;
#3789 = CARTESIAN_POINT ( 'NONE',  ( 18.14488609917747652, 6.993670804558928644, -231.4804853770579882 ) ) ;
#3790 = CARTESIAN_POINT ( 'NONE',  ( -5.383332542724544645, 15.12651309054520432, -231.5699995578976313 ) ) ;
#3791 = CARTESIAN_POINT ( 'NONE',  ( -21.80000000000008242, 0.000000000000000000, 78.50000000000000000 ) ) ;
#3792 = CARTESIAN_POINT ( 'NONE',  ( 17.35243190875273811, 16.67741344734974263, -230.5744436858935558 ) ) ;
#3793 = CARTESIAN_POINT ( 'NONE',  ( 5.701450259358237460, -28.73672391946437088, -229.2085834618566196 ) ) ;
#3794 = ORIENTED_EDGE ( 'NONE', *, *, #11758, .T. ) ;
#3795 = CIRCLE ( 'NONE', #21027, 2.000000000000001776 ) ;
#3796 = CARTESIAN_POINT ( 'NONE',  ( -4.080659539198054020, 15.43130099126780408, -228.8058965243247656 ) ) ;
#3797 = CARTESIAN_POINT ( 'NONE',  ( -18.94009481283715957, 3.115208415279245191, -230.3622730452590588 ) ) ;
#3798 = CARTESIAN_POINT ( 'NONE',  ( -27.17783334270200157, 15.20409188923851751, -223.6555185980277258 ) ) ;
#3799 = CARTESIAN_POINT ( 'NONE',  ( -15.17770002056818868, -9.429316640439420638, -220.2566215541993699 ) ) ;
#3800 = DIRECTION ( 'NONE',  ( 0.000000000000000000, 1.000000000000000000, -0.000000000000000000 ) ) ;
#3801 = ORIENTED_EDGE ( 'NONE', *, *, #7097, .T. ) ;
#3802 = CARTESIAN_POINT ( 'NONE',  ( 25.02650711521362936, 17.58144575069911042, -223.6165279156031431 ) ) ;
#3803 = CARTESIAN_POINT ( 'NONE',  ( 1.866975752136456279, -28.95217164724439840, -224.5474425503401221 ) ) ;
#3804 = CARTESIAN_POINT ( 'NONE',  ( 19.72515656911863147, 14.02277373989196541, -218.0718040828188009 ) ) ;
#3805 = CARTESIAN_POINT ( 'NONE',  ( -10.30050448363967419, 10.07750059423401190, -220.1837019037183723 ) ) ;
#3806 = B_SPLINE_CURVE_WITH_KNOTS ( 'NONE', 3,
 ( #6756, #8666, #5160, #4944, #3026, #8563, #18578, #20235, #10023, #20123, #4831, #11928, #15427, #6865, #3140, #11590, #15529, #1790, #18462, #9913, #16776, #8224, #6522, #13392, #8335, #11820, #12378, #3809, #17662, #19008, #17325, #2124, #17779, #10462, #8895, #13961, #552 ),
 .UNSPECIFIED., .F., .F.,
 ( 4, 1, 1, 1, 1, 2, 2, 1, 1, 1, 1, 1, 2, 2, 1, 1, 1, 1, 1, 2, 2, 1, 1, 1, 1, 1, 2, 4 ),
 ( 0.000000000000000000, 0.06250000000000048572, 0.09375000000000069389, 0.1093750000000008049, 0.1171875000000008604, 0.1210937500000009159, 0.1250000000000009714, 0.1875000000000012212, 0.2187500000000013600, 0.2343750000000014433, 0.2421875000000014710, 0.2460937500000014710, 0.2480468750000014710, 0.2500000000000014988, 0.3125000000000016653, 0.3437500000000017208, 0.3593750000000017764, 0.3671875000000017764, 0.3710937500000017764, 0.3730468750000017208, 0.3750000000000016653, 0.4375000000000008882, 0.4687500000000004996, 0.4843750000000002776, 0.4921875000000001665, 0.4960937500000000555, 0.4980468750000000555, 0.5000000000000000000 ),
 .UNSPECIFIED. ) ;
#3807 = CARTESIAN_POINT ( 'NONE',  ( 17.98589043827631428, 2.945998030785370592, -233.4030907785035538 ) ) ;
#3808 = CARTESIAN_POINT ( 'NONE',  ( 4.301648988406530094, 13.23079486486395240, -223.2766268961034655 ) ) ;
#3809 = CARTESIAN_POINT ( 'NONE',  ( -8.674798497629360838, 6.539635590297948831, 91.99999999999997158 ) ) ;
#3810 = CARTESIAN_POINT ( 'NONE',  ( -5.240862053303020573, -11.96147391800445270, -224.1453450823045443 ) ) ;
#3811 = CARTESIAN_POINT ( 'NONE',  ( 12.84024077373997841, -14.50125846907313054, -216.8496453050001946 ) ) ;
#3812 = DIRECTION ( 'NONE',  ( 0.000000000000000000, 0.000000000000000000, -1.000000000000000000 ) ) ;
#3813 = FACE_OUTER_BOUND ( 'NONE', #2116, .T. ) ;
#3814 = CARTESIAN_POINT ( 'NONE',  ( -12.38801939673351704, 9.361418580567464787, -232.8075769614211765 ) ) ;
#3815 = CARTESIAN_POINT ( 'NONE',  ( -15.27576489228250090, -6.235258113955679526, -227.2120396213316553 ) ) ;
#3816 = CARTESIAN_POINT ( 'NONE',  ( 20.18206873099720156, 1.748383523995667987, -234.4526011791959661 ) ) ;
#3817 = CARTESIAN_POINT ( 'NONE',  ( -0.5888410438786807477, 14.99789765555501475, -227.7044550383138244 ) ) ;
#3818 = CARTESIAN_POINT ( 'NONE',  ( 5.064106757301036765, 16.06517852189101703, -221.6413221086847329 ) ) ;
#3819 = ORIENTED_EDGE ( 'NONE', *, *, #17680, .F. ) ;
#3820 = CARTESIAN_POINT ( 'NONE',  ( 11.96323484613444599, -17.37820513000257350, -215.5071828020160183 ) ) ;
#3821 = EDGE_LOOP ( 'NONE', ( #17497, #17029, #20739, #5281 ) ) ;
#3822 = AXIS2_PLACEMENT_3D ( 'NONE', #18252, #2814, #13071 ) ;
#3823 = CARTESIAN_POINT ( 'NONE',  ( 23.49048926389013658, 9.645778135078892035, -218.7307869890797463 ) ) ;
#3824 = CARTESIAN_POINT ( 'NONE',  ( -10.01410430826631170, 16.10970239316000630, -233.6135099156378203 ) ) ;
#3825 = CARTESIAN_POINT ( 'NONE',  ( -16.48591407464216729, 7.092323989942422635, -218.8909951703408012 ) ) ;
#3826 = CARTESIAN_POINT ( 'NONE',  ( -20.63475909113443763, -3.483688486440585486, -233.7225001494461480 ) ) ;
#3827 = CARTESIAN_POINT ( 'NONE',  ( -14.07917727715460821, 7.534853284453274291, -218.6337090155677458 ) ) ;
#3828 = PLANE ( 'NONE',  #1497 ) ;
#3829 = DIRECTION ( 'NONE',  ( -1.000000000000000000, 0.000000000000000000, 0.000000000000000000 ) ) ;
#3830 = DIRECTION ( 'NONE',  ( 1.000000000000000000, 0.000000000000000000, 0.000000000000000000 ) ) ;
#3831 = CARTESIAN_POINT ( 'NONE',  ( -18.92390258637512090, 12.75887082072172163, -230.9970325548277970 ) ) ;
#3832 = CARTESIAN_POINT ( 'NONE',  ( 24.19672885113291727, 10.99915907690374439, -233.6834417629405891 ) ) ;
#3833 = CARTESIAN_POINT ( 'NONE',  ( -28.99926036811508467, 3.909990568804979194, -228.9613767892386988 ) ) ;
#3834 = SHAPE_REPRESENTATION ( 'Removable  Lid', ( #6677 ), #10599 ) ;
#3835 = CARTESIAN_POINT ( 'NONE',  ( -26.48368569639269055, -17.40725828600530534, -221.7871577296580199 ) ) ;
#3836 = CARTESIAN_POINT ( 'NONE',  ( -27.10757994293576800, -10.52107906247675473, -229.7403242048749519 ) ) ;
#3837 = CARTESIAN_POINT ( 'NONE',  ( -11.23881320317003407, 15.84151802331611236, -234.2799649731619809 ) ) ;
#3838 = CARTESIAN_POINT ( 'NONE',  ( -9.625604265899946554, -19.21123364792547505, -233.9327940972253259 ) ) ;
#3839 = CARTESIAN_POINT ( 'NONE',  ( 4.603870848087811218, 30.13529352683433515, -225.9623629403671430 ) ) ;
#3840 = CARTESIAN_POINT ( 'NONE',  ( 5.535251771770903773, -29.91249465213552128, -219.7039649384792028 ) ) ;
#3841 = DIRECTION ( 'NONE',  ( 0.000000000000000000, 0.000000000000000000, -1.000000000000000000 ) ) ;
#3842 = EDGE_CURVE ( 'NONE', #10586, #16331, #3766, .T. ) ;
#3843 = CARTESIAN_POINT ( 'NONE',  ( -22.10934047915427314, 0.9940043559354312386, -216.9999999999999716 ) ) ;
#3844 =( NAMED_UNIT ( * ) SI_UNIT ( $, .STERADIAN. ) SOLID_ANGLE_UNIT ( ) );
#3845 = CARTESIAN_POINT ( 'NONE',  ( -8.467651734177735534, 23.23776955534497546, -231.2693664226804913 ) ) ;
#3846 = CARTESIAN_POINT ( 'NONE',  ( -20.71192633727912380, 6.339941255257877550, -217.2401662359725094 ) ) ;
#3847 = CARTESIAN_POINT ( 'NONE',  ( 22.18132842682159733, 5.591149267797686839, -232.0584733989884114 ) ) ;
#3848 = CARTESIAN_POINT ( 'NONE',  ( 14.87635807518583775, 11.13002414557121789, -232.1789382499626981 ) ) ;
#3849 = CARTESIAN_POINT ( 'NONE',  ( -11.03528491614390994, -18.43141318057359612, -232.7233776306152038 ) ) ;
#3850 = CARTESIAN_POINT ( 'NONE',  ( 15.79748369401691122, 19.19631269170049137, -215.0096632418193963 ) ) ;
#3851 = FACE_OUTER_BOUND ( 'NONE', #11943, .T. ) ;
#3852 = CARTESIAN_POINT ( 'NONE',  ( -9.794218246645117532, -15.26311849320921255, -215.4893187949746505 ) ) ;
#3853 = CARTESIAN_POINT ( 'NONE',  ( -4.130417896617784912, 16.21758012034559826, -229.8171973319304584 ) ) ;
#3854 = CARTESIAN_POINT ( 'NONE',  ( 22.20554449732931346, 18.01468431515759860, -218.9348803756412849 ) ) ;
#3855 = CARTESIAN_POINT ( 'NONE',  ( -12.96364545172611571, 10.77137376900670063, -221.1208843751685720 ) ) ;
#3856 = CARTESIAN_POINT ( 'NONE',  ( -4.877547524699579640, 12.94924496403020697, -219.3991240521417581 ) ) ;
#3857 = CARTESIAN_POINT ( 'NONE',  ( 14.68015846516680867, 2.651775288685355836, -224.1317433549420173 ) ) ;
#3858 = CARTESIAN_POINT ( 'NONE',  ( 8.129749879387842881, -22.89596468334109147, -230.6606593278197295 ) ) ;
#3859 = ORIENTED_EDGE ( 'NONE', *, *, #13136, .F. ) ;
#3860 = CARTESIAN_POINT ( 'NONE',  ( 10.08089751255479527, -9.763210684072014089, -226.4220581413412390 ) ) ;
#3861 = CARTESIAN_POINT ( 'NONE',  ( -0.3589900283600636066, 18.35437183075527656, -220.3960288481451357 ) ) ;
#3862 = VERTEX_POINT ( 'NONE', #10651 ) ;
#3863 = CARTESIAN_POINT ( 'NONE',  ( 0.000000000000000000, 0.000000000000000000, -75.00000000000000000 ) ) ;
#3864 = CARTESIAN_POINT ( 'NONE',  ( 10.55627441269396094, 10.31758739525044888, -223.1990319438957613 ) ) ;
#3865 = CARTESIAN_POINT ( 'NONE',  ( 17.43540344723615476, -3.335533435063737340, -230.8961756483947738 ) ) ;
#3866 = CARTESIAN_POINT ( 'NONE',  ( -15.19144047750087267, -10.24270553329939304, -232.4311702607364793 ) ) ;
#3867 = CARTESIAN_POINT ( 'NONE',  ( -6.163092920833200594, -27.00835405423771007, -232.1022292408408987 ) ) ;
#3868 = CARTESIAN_POINT ( 'NONE',  ( -2.723069588102707606, 15.58614045890443833, -225.0254611642426141 ) ) ;
#3869 = DIRECTION ( 'NONE',  ( 0.000000000000000000, 0.000000000000000000, -1.000000000000000000 ) ) ;
#3870 = CARTESIAN_POINT ( 'NONE',  ( 24.96615890023450035, 5.871290975262302148, -218.1661911638112201 ) ) ;
#3871 = CARTESIAN_POINT ( 'NONE',  ( -6.474151797443945533, 21.29193859232740138, -215.9573456447696458 ) ) ;
#3872 = CARTESIAN_POINT ( 'NONE',  ( -9.746008880186941781, 12.96562886885531896, -220.1990846131056401 ) ) ;
#3873 = VERTEX_POINT ( 'NONE', #67 ) ;
#3874 = CARTESIAN_POINT ( 'NONE',  ( 6.771176146757415637, 15.60014285904435027, -218.3493856697694753 ) ) ;
#3875 = CARTESIAN_POINT ( 'NONE',  ( -23.52458685063474420, 4.195399146287285497, -230.7490123595086970 ) ) ;
#3876 = CARTESIAN_POINT ( 'NONE',  ( 16.67941620816951698, 4.093285459228785506, -217.1675623234529269 ) ) ;
#3877 = CARTESIAN_POINT ( 'NONE',  ( 13.38323588254664642, -24.59169381177348157, -229.6955247737395780 ) ) ;
#3878 = CARTESIAN_POINT ( 'NONE',  ( 4.100000000000000533, 0.000000000000000000, -75.00000000000000000 ) ) ;
#3879 = EDGE_LOOP ( 'NONE', ( #907, #18094 ) ) ;
#3880 = EDGE_CURVE ( 'NONE', #10146, #945, #515, .T. ) ;
#3881 = CARTESIAN_POINT ( 'NONE',  ( 9.333020543840051531, 16.91085096921651143, -217.7308990335875762 ) ) ;
#3882 = CARTESIAN_POINT ( 'NONE',  ( -13.09367826499460818, -1.871088059101057244, -230.2970504731880510 ) ) ;
#3883 = DIRECTION ( 'NONE',  ( 0.000000000000000000, 0.000000000000000000, -1.000000000000000000 ) ) ;
#3884 = CARTESIAN_POINT ( 'NONE',  ( 18.54610009393809023, 0.6523581019769808531, -231.1787333216317677 ) ) ;
#3885 = CARTESIAN_POINT ( 'NONE',  ( 3.342529885312644833, -17.78621320651278737, -216.7788622297345853 ) ) ;
#3886 = SHAPE_REPRESENTATION_RELATIONSHIP ( 'NONE' , 'NONE' ,  #8462, #21175 ) ;
#3887 = CARTESIAN_POINT ( 'NONE',  ( -9.517741096562200909, 20.63709896626785678, -234.1036702156204967 ) ) ;
#3888 = CARTESIAN_POINT ( 'NONE',  ( -24.33894786102607455, 16.69464852328507831, -227.6320542475859554 ) ) ;
#3889 = ORIENTED_EDGE ( 'NONE', *, *, #8253, .F. ) ;
#3890 = CARTESIAN_POINT ( 'NONE',  ( -21.93900267957129557, 7.862893636934532360, -233.4951761057262161 ) ) ;
#3891 = CARTESIAN_POINT ( 'NONE',  ( -19.75205891382245227, -22.10994567413457546, -223.7241504221178729 ) ) ;
#3892 = CARTESIAN_POINT ( 'NONE',  ( -24.86551311171973566, -2.609124161958199739, -9.659280632943737288 ) ) ;
#3893 = EDGE_CURVE ( 'NONE', #17518, #5014, #10425, .T. ) ;
#3894 = CARTESIAN_POINT ( 'NONE',  ( 0.000000000000000000, 0.000000000000000000, -78.50000000000000000 ) ) ;
#3895 = CARTESIAN_POINT ( 'NONE',  ( -14.07917727715460821, 7.534853284453274291, -218.6337090155677458 ) ) ;
#3896 = CARTESIAN_POINT ( 'NONE',  ( 0.3659801352207852077, -13.50984377477715093, -221.1746532791751463 ) ) ;
#3897 = FILL_AREA_STYLE_COLOUR ( '', #6324 ) ;
#3898 = LINE ( 'NONE', #17536, #9470 ) ;
#3899 = CARTESIAN_POINT ( 'NONE',  ( 15.33128967029630729, 6.504525012335983902, -229.0514072561169883 ) ) ;
#3900 = CARTESIAN_POINT ( 'NONE',  ( -19.40752943788874774, 15.61499612050012864, -234.7624367253776541 ) ) ;
#3901 = CIRCLE ( 'NONE', #17927, 10.00000000000000000 ) ;
#3902 = CARTESIAN_POINT ( 'NONE',  ( 0.000000000000000000, 23.00000000000006040, 69.99999999999998579 ) ) ;
#3903 = CARTESIAN_POINT ( 'NONE',  ( 12.00334754111224100, 12.62951371569041115, -228.5814949098771649 ) ) ;
#3904 = CARTESIAN_POINT ( 'NONE',  ( -1.178362239076253370, -26.64461120719161613, -230.8441371545519019 ) ) ;
#3905 = ORIENTED_EDGE ( 'NONE', *, *, #7475, .T. ) ;
#3906 = CARTESIAN_POINT ( 'NONE',  ( 2.703362520412529779, 29.60004130108520215, -225.6165589735000481 ) ) ;
#3907 = CARTESIAN_POINT ( 'NONE',  ( -18.59263364681495290, 22.28600439725833482, -224.9897462721271779 ) ) ;
#3908 = CARTESIAN_POINT ( 'NONE',  ( -13.63442241228529994, 1.608023091903783008, -219.2326980015357094 ) ) ;
#3909 = ORIENTED_EDGE ( 'NONE', *, *, #2466, .F. ) ;
#3910 = CARTESIAN_POINT ( 'NONE',  ( -10.61621529918308227, -15.65610094335291969, -220.0975530242428420 ) ) ;
#3911 = CARTESIAN_POINT ( 'NONE',  ( 0.000000000000000000, 0.000000000000000000, -60.00000000000000000 ) ) ;
#3912 = ORIENTED_EDGE ( 'NONE', *, *, #3073, .F. ) ;
#3913 = CARTESIAN_POINT ( 'NONE',  ( -16.15126510923403202, -0.4755054218165427615, -219.3066569788202571 ) ) ;
#3914 = CARTESIAN_POINT ( 'NONE',  ( 3.323726671003152777, -15.99176757603385823, -228.1400570273458186 ) ) ;
#3915 = CARTESIAN_POINT ( 'NONE',  ( 23.04897566969193079, 17.95862962700741861, -223.6438515760422661 ) ) ;
#3916 = CARTESIAN_POINT ( 'NONE',  ( -2.934221234790329369, 15.07857928364152222, -230.9558365497803720 ) ) ;
#3917 = CARTESIAN_POINT ( 'NONE',  ( 16.67941620816951698, 4.093285459228785506, -217.1675623234529269 ) ) ;
#3918 = EDGE_CURVE ( 'NONE', #7331, #9583, #9301, .T. ) ;
#3919 = CARTESIAN_POINT ( 'NONE',  ( 10.50530447320976535, 20.19629329636330084, -217.1354359361034767 ) ) ;
#3920 = DIRECTION ( 'NONE',  ( 0.000000000000000000, 0.000000000000000000, -1.000000000000000000 ) ) ;
#3921 = CARTESIAN_POINT ( 'NONE',  ( -5.804961988600464196, -12.67915086496026511, -228.7923277404792088 ) ) ;
#3922 = CARTESIAN_POINT ( 'NONE',  ( 25.83609367470520723, -15.13481494965009411, -225.4685613576401124 ) ) ;
#3923 = B_SPLINE_CURVE_WITH_KNOTS ( 'NONE', 3,
 ( #19992, #11347, #18218, #13254, #7972, #2777, #21906, #20098, #8308, #18436, #2999, #1326, #14839, #6049, #2884, #16746, #9661, #15176 ),
 .UNSPECIFIED., .F., .F.,
 ( 4, 2, 2, 2, 2, 2, 2, 2, 4 ),
 ( 4.470280076681872704E-18, 0.0004125412386659448559, 0.0008250824773318852666, 0.001237623715997825677, 0.001650164954663766196, 0.002062706193329706499, 0.002475247431995646584, 0.002887788670661587103, 0.003300329909327527622 ),
 .UNSPECIFIED. ) ;
#3924 = DIRECTION ( 'NONE',  ( -1.000000000000000000, 0.000000000000000000, -0.000000000000000000 ) ) ;
#3925 = CARTESIAN_POINT ( 'NONE',  ( 0.000000000000000000, 0.000000000000000000, 75.00000000000000000 ) ) ;
#3926 = CARTESIAN_POINT ( 'NONE',  ( -28.12586305337175219, 12.75764838638491305, -230.3810511299127768 ) ) ;
#3927 = CARTESIAN_POINT ( 'NONE',  ( -16.27785121718144623, -3.187812258433146084, -227.1052622255949132 ) ) ;
#3928 = CARTESIAN_POINT ( 'NONE',  ( -13.70798801564395752, 13.71024986321384809, -218.3360451569033955 ) ) ;
#3929 = CARTESIAN_POINT ( 'NONE',  ( 25.62718606866737403, 13.33219119508369310, -230.9315691959737933 ) ) ;
#3930 = CARTESIAN_POINT ( 'NONE',  ( 5.909674498212842408, 15.76475534640655773, -228.4922217450045139 ) ) ;
#3931 = ORIENTED_EDGE ( 'NONE', *, *, #17519, .T. ) ;
#3932 = CARTESIAN_POINT ( 'NONE',  ( 10.87654225111433526, -5.446269956799608458, -227.9455542281931741 ) ) ;
#3933 = ORIENTED_EDGE ( 'NONE', *, *, #15250, .T. ) ;
#3934 = CARTESIAN_POINT ( 'NONE',  ( 18.60971343765040942, 2.368090295052050820, -218.6871071987073094 ) ) ;
#3935 = CARTESIAN_POINT ( 'NONE',  ( -17.94782256308196366, 19.07396065564992682, -232.7143578890335220 ) ) ;
#3936 = CARTESIAN_POINT ( 'NONE',  ( -13.31245686955614005, 26.96290519511623174, -230.1796856776773836 ) ) ;
#3937 = CARTESIAN_POINT ( 'NONE',  ( -14.01584329375060456, -3.774282517739922405, -220.6818330080343173 ) ) ;
#3938 = CARTESIAN_POINT ( 'NONE',  ( -27.90314475660494153, 12.48829126175061077, -223.3300566725355338 ) ) ;
#3939 = CARTESIAN_POINT ( 'NONE',  ( 1.387778780781446180E-13, -19.80000000000006111, -78.50000000000000000 ) ) ;
#3940 = CARTESIAN_POINT ( 'NONE',  ( 14.64930099072384095, -2.233284345536625803, -226.6630761355773984 ) ) ;
#3941 = CARTESIAN_POINT ( 'NONE',  ( -10.07004052286948337, 22.64471483900350179, -217.4645417110143626 ) ) ;
#3942 = CARTESIAN_POINT ( 'NONE',  ( 13.85822045549773129, -1.469587484828172919, -226.8778453516271156 ) ) ;
#3943 = CARTESIAN_POINT ( 'NONE',  ( -17.84981083811007707, 0.8485253248287054628, -231.8041300026935119 ) ) ;
#3944 = CARTESIAN_POINT ( 'NONE',  ( 12.18657022793382794, 26.76558097653315471, -221.8882195427397335 ) ) ;
#3945 = CARTESIAN_POINT ( 'NONE',  ( -13.44605823798860200, -7.860403065310468840, -219.7865185367595586 ) ) ;
#3946 = CARTESIAN_POINT ( 'NONE',  ( 5.248013545904832711, 18.51731616863089158, -219.3673127389703552 ) ) ;
#3947 = CARTESIAN_POINT ( 'NONE',  ( -1.643553855084622928, -13.05119293000219294, -222.7191902239112551 ) ) ;
#3948 = CARTESIAN_POINT ( 'NONE',  ( 10.66614775643814994, 26.29080367171353672, -230.0818785118670178 ) ) ;
#3949 = CARTESIAN_POINT ( 'NONE',  ( 10.15560415551905749, -12.94826033684588928, -216.3500876866647502 ) ) ;
#3950 = CARTESIAN_POINT ( 'NONE',  ( 0.000000000000000000, 0.000000000000000000, -77.51594804401857175 ) ) ;
#3951 = CARTESIAN_POINT ( 'NONE',  ( -19.65084584916038324, 18.01805631773661176, -219.5040736310571106 ) ) ;
#3952 = DIRECTION ( 'NONE',  ( -1.000000000000000000, 0.000000000000000000, 0.000000000000000000 ) ) ;
#3953 = CARTESIAN_POINT ( 'NONE',  ( 14.58943670538545412, -3.864781073802256550, -230.4050158740328129 ) ) ;
#3954 = CARTESIAN_POINT ( 'NONE',  ( 3.746955526231565248, 25.82691596581962656, -220.7780764774678062 ) ) ;
#3955 = CARTESIAN_POINT ( 'NONE',  ( -26.19327040236159831, 13.44417515682194875, -223.7810975255189874 ) ) ;
#3956 = CARTESIAN_POINT ( 'NONE',  ( 25.69300549816939494, 5.947472783069708946, -230.6131061331718115 ) ) ;
#3957 = CARTESIAN_POINT ( 'NONE',  ( -15.02551512915570697, -20.93241195546420741, -218.9083119944682778 ) ) ;
#3958 = CARTESIAN_POINT ( 'NONE',  ( 20.82555317450757215, 14.06078233701296476, -215.4201375757437802 ) ) ;
#3959 = DIRECTION ( 'NONE',  ( -0.000000000000000000, 0.000000000000000000, -1.000000000000000000 ) ) ;
#3960 = CARTESIAN_POINT ( 'NONE',  ( -6.645226799955220365, -27.24439832571371767, -217.1032720093393493 ) ) ;
#3961 = CARTESIAN_POINT ( 'NONE',  ( -9.988594796049140356, 11.34066464990972811, -226.6453149279956563 ) ) ;
#3962 = CARTESIAN_POINT ( 'NONE',  ( 12.95792863868717149, 16.83236386576623644, -216.3406066345214356 ) ) ;
#3963 = CARTESIAN_POINT ( 'NONE',  ( -25.17056316833229701, 11.10725809642625705, -227.0225660235207386 ) ) ;
#3964 = EDGE_CURVE ( 'NONE', #17015, #11981, #7055, .T. ) ;
#3965 = CARTESIAN_POINT ( 'NONE',  ( -12.98662328632235585, 28.83726371277012035, -223.5970274767108776 ) ) ;
#3966 = CIRCLE ( 'NONE', #19425, 13.12488928717151637 ) ;
#3967 = CARTESIAN_POINT ( 'NONE',  ( 17.47660375112063491, 0.1533180678384444551, -220.6249646429494931 ) ) ;
#3968 = CARTESIAN_POINT ( 'NONE',  ( 7.144583572002897398, -18.19063289417396945, -230.4059351064080658 ) ) ;
#3969 = ORIENTED_EDGE ( 'NONE', *, *, #8054, .F. ) ;
#3970 = CARTESIAN_POINT ( 'NONE',  ( 13.66436340482409761, -13.84785698770488871, -232.6553000701566134 ) ) ;
#3971 = CARTESIAN_POINT ( 'NONE',  ( -2.806347010929339802, 19.90767250424812573, -230.9206976900916004 ) ) ;
#3972 = DIRECTION ( 'NONE',  ( 4.408728476930457445E-15, -1.000000000000000000, 0.000000000000000000 ) ) ;
#3973 = CARTESIAN_POINT ( 'NONE',  ( 16.07305932912010960, 0.9253679043337685872, -229.0409936706996064 ) ) ;
#3974 = CARTESIAN_POINT ( 'NONE',  ( -22.30463520409893263, -0.6981587008078518064, -233.9491726243120127 ) ) ;
#3975 = CARTESIAN_POINT ( 'NONE',  ( -22.51170993270524789, -14.32174306031543054, -231.7292175355062795 ) ) ;
#3976 = CARTESIAN_POINT ( 'NONE',  ( -7.832594822155400927, -23.57318293858060088, -216.4298491688572028 ) ) ;
#3977 = CARTESIAN_POINT ( 'NONE',  ( -6.901278853520646628, 15.41233971300566807, -220.5972764307651346 ) ) ;
#3978 = FACE_OUTER_BOUND ( 'NONE', #4905, .T. ) ;
#3979 = CARTESIAN_POINT ( 'NONE',  ( -27.12694304224540076, 7.756125161462346540, -217.3817363082233101 ) ) ;
#3980 = CARTESIAN_POINT ( 'NONE',  ( -2.958555384449997661, 13.07587799061801093, -222.7767538261418565 ) ) ;
#3981 = CARTESIAN_POINT ( 'NONE',  ( 3.746955526231565248, 25.82691596581962656, -220.7780764774678062 ) ) ;
#3982 = ORIENTED_EDGE ( 'NONE', *, *, #7373, .F. ) ;
#3983 = CARTESIAN_POINT ( 'NONE',  ( 5.702651035983461902, 12.42242820409033222, -224.7304266323218656 ) ) ;
#3984 = CARTESIAN_POINT ( 'NONE',  ( -15.83894155097017631, 1.950284868793920712, -224.5615909987450038 ) ) ;
#3985 = CARTESIAN_POINT ( 'NONE',  ( 30.57915561709945251, 3.468229287067555067, -223.8876084027091906 ) ) ;
#3986 = CARTESIAN_POINT ( 'NONE',  ( 19.57710422433000019, -21.48596639614413562, -228.6055549924913635 ) ) ;
#3987 = DIRECTION ( 'NONE',  ( -0.000000000000000000, 0.000000000000000000, -1.000000000000000000 ) ) ;
#3988 = ORIENTED_EDGE ( 'NONE', *, *, #13826, .F. ) ;
#3989 = CARTESIAN_POINT ( 'NONE',  ( 8.689059922489732912, 15.18271246186214363, -218.7354841152034908 ) ) ;
#3990 = CARTESIAN_POINT ( 'NONE',  ( 26.08609146265030176, -9.082777145696592669, -223.3125241607380360 ) ) ;
#3991 = CARTESIAN_POINT ( 'NONE',  ( 28.78651053433536333, -0.9604905981993369091, -227.3547688931310233 ) ) ;
#3992 = CARTESIAN_POINT ( 'NONE',  ( 6.374306683232226156, -13.38367253400339330, -219.9651431149896723 ) ) ;
#3993 =( NAMED_UNIT ( * ) SI_UNIT ( $, .STERADIAN. ) SOLID_ANGLE_UNIT ( ) );
#3994 = CARTESIAN_POINT ( 'NONE',  ( -17.17400284685640344, 24.63223427531467280, -220.6313524368512162 ) ) ;
#3995 = CARTESIAN_POINT ( 'NONE',  ( -7.812160407601123069, 10.19183344000749081, -223.8148904943605828 ) ) ;
#3996 = ORIENTED_EDGE ( 'NONE', *, *, #6636, .F. ) ;
#3997 = CARTESIAN_POINT ( 'NONE',  ( -11.46843428684449151, 6.508406145394057596, -225.7212143570321814 ) ) ;
#3998 = CARTESIAN_POINT ( 'NONE',  ( -23.08212926897555306, -14.71479305961103101, -218.7697472404056214 ) ) ;
#3999 = DIRECTION ( 'NONE',  ( -0.000000000000000000, -0.000000000000000000, -1.000000000000000000 ) ) ;
#4000 = FACE_OUTER_BOUND ( 'NONE', #15773, .T. ) ;
#4001 = CARTESIAN_POINT ( 'NONE',  ( -13.93333636822611155, 3.327141996558931947, -221.4468162587888287 ) ) ;
#4002 = CARTESIAN_POINT ( 'NONE',  ( 9.678950682101415737, -24.51930918146190663, -231.5088683414745105 ) ) ;
#4003 = EDGE_CURVE ( 'NONE', #12254, #20879, #20779, .T. ) ;
#4004 = CARTESIAN_POINT ( 'NONE',  ( -28.13472254077564116, 12.33996625515159629, -224.9141344439281909 ) ) ;
#4005 = AXIS2_PLACEMENT_3D ( 'NONE', #16157, #5901, #12988 ) ;
#4006 = CARTESIAN_POINT ( 'NONE',  ( 14.68130101653174613, 6.427210486143660084, -228.0153742661088074 ) ) ;
#4007 = CARTESIAN_POINT ( 'NONE',  ( -8.716816145717144693, 12.22834664005217675, -231.7124508691059646 ) ) ;
#4008 = DIRECTION ( 'NONE',  ( -1.000000000000000000, 0.000000000000000000, 0.000000000000000000 ) ) ;
#4009 = CARTESIAN_POINT ( 'NONE',  ( 18.90025403853754327, 17.70150481658638952, -229.5234643039372315 ) ) ;
#4010 = CARTESIAN_POINT ( 'NONE',  ( 1.038689920556553847, -18.98022482494055652, -217.9213632692622866 ) ) ;
#4011 = ORIENTED_EDGE ( 'NONE', *, *, #12403, .T. ) ;
#4012 = CARTESIAN_POINT ( 'NONE',  ( -0.3197916200495275474, 16.38897215927557482, -229.9606066735827028 ) ) ;
#4013 = CARTESIAN_POINT ( 'NONE',  ( -18.36252859017411510, 21.06344830687906367, -228.5073589488702623 ) ) ;
#4014 = CARTESIAN_POINT ( 'NONE',  ( -14.83806045519817829, 13.18806197935771074, -233.4179411789645542 ) ) ;
#4015 = AXIS2_PLACEMENT_3D ( 'NONE', #21200, #5574, #10760 ) ;
#4016 = CARTESIAN_POINT ( 'NONE',  ( -17.87876569233342749, -13.82805272504658944, -230.9569051913176168 ) ) ;
#4017 = DIRECTION ( 'NONE',  ( 1.000000000000000000, 0.000000000000000000, 0.000000000000000000 ) ) ;
#4018 = VERTEX_POINT ( 'NONE', #1861 ) ;
#4019 = CARTESIAN_POINT ( 'NONE',  ( -17.88126539071149779, 5.766250685202066961, -232.9050303536861293 ) ) ;
#4020 = CARTESIAN_POINT ( 'NONE',  ( 3.208289162541382300, -18.46136333555241293, -230.6641274008648850 ) ) ;
#4021 = CARTESIAN_POINT ( 'NONE',  ( 24.57222455393806015, 12.08236629421828212, -229.7319216558644541 ) ) ;
#4022 = CARTESIAN_POINT ( 'NONE',  ( 5.141746912158045468, 22.01688500372448232, -216.6678693612369386 ) ) ;
#4023 = UNCERTAINTY_MEASURE_WITH_UNIT (LENGTH_MEASURE( 1.000000000000000082E-05 ), #4912, 'distance_accuracy_value', 'NONE');
#4024 = CIRCLE ( 'NONE', #16608, 19.63401512838747820 ) ;
#4025 = CARTESIAN_POINT ( 'NONE',  ( -27.11599398522282911, 10.60460483532474996, -224.7310548435675912 ) ) ;
#4026 = CARTESIAN_POINT ( 'NONE',  ( 14.28815361401014172, 13.86049093364188778, -216.0585456615740156 ) ) ;
#4027 = AXIS2_PLACEMENT_3D ( 'NONE', #12369, #14064, #14178 ) ;
#4028 = CARTESIAN_POINT ( 'NONE',  ( 13.03557269046774714, 7.519834803053426775, -226.9490612297269081 ) ) ;
#4029 = DIRECTION ( 'NONE',  ( 1.000000000000000000, 6.982962677686266711E-15, 0.000000000000000000 ) ) ;
#4030 = CARTESIAN_POINT ( 'NONE',  ( -5.279374154171231126, -12.28263746854076466, -222.5283095625445640 ) ) ;
#4031 = CARTESIAN_POINT ( 'NONE',  ( 8.115778909262310492, -29.92983049028717346, -224.5060555478150377 ) ) ;
#4032 = LINE ( 'NONE', #21029, #9543 ) ;
#4033 = DIRECTION ( 'NONE',  ( 0.000000000000000000, 0.000000000000000000, -1.000000000000000000 ) ) ;
#4034 = CARTESIAN_POINT ( 'NONE',  ( -10.49339404011726984, 12.66576824096800991, -217.2681947942554643 ) ) ;
#4035 = CARTESIAN_POINT ( 'NONE',  ( -16.47483915600249205, -3.991485801086211538, -222.0851216934102297 ) ) ;
#4036 = CARTESIAN_POINT ( 'NONE',  ( -21.23733589435050817, 17.25275849955597351, -229.9547908233139708 ) ) ;
#4037 = CARTESIAN_POINT ( 'NONE',  ( 12.08198696763335178, 15.54678077493410981, -216.6084679670902631 ) ) ;
#4038 = CARTESIAN_POINT ( 'NONE',  ( -1.946052076048385482, 22.23149728939677061, -232.8927760318659068 ) ) ;
#4039 = ORIENTED_EDGE ( 'NONE', *, *, #13717, .T. ) ;
#4040 = CARTESIAN_POINT ( 'NONE',  ( 25.79180107113126397, -16.09695083256378112, -231.0225534820104656 ) ) ;
#4041 = CARTESIAN_POINT ( 'NONE',  ( 24.57222455393806015, 12.08236629421828212, -229.7319216558644541 ) ) ;
#4042 = TOROIDAL_SURFACE ( 'NONE', #8734, 22.56777165119825668, 5.000000000000000000 ) ;
#4043 = AXIS2_PLACEMENT_3D ( 'NONE', #13177, #18133, #21596 ) ;
#4044 = CARTESIAN_POINT ( 'NONE',  ( 0.6332696906856497554, 18.74964962670039625, -234.8596399859513042 ) ) ;
#4045 = CARTESIAN_POINT ( 'NONE',  ( -16.28135616697389310, 20.98764039357472200, -216.9434553755565958 ) ) ;
#4046 = CARTESIAN_POINT ( 'NONE',  ( -29.05925532287432489, -3.238226816112620199, -230.1495230746535867 ) ) ;
#4047 = EDGE_CURVE ( 'NONE', #15083, #21835, #16844, .T. ) ;
#4048 = CARTESIAN_POINT ( 'NONE',  ( -12.78558550453068854, 7.693178343823584342, -230.0800953344970878 ) ) ;
#4049 = CARTESIAN_POINT ( 'NONE',  ( -0.06328415631827169485, -14.50030254718124390, 92.99999999999998579 ) ) ;
#4050 = EDGE_CURVE ( 'NONE', #2515, #1930, #10862, .T. ) ;
#4051 = CARTESIAN_POINT ( 'NONE',  ( -17.50000000000000355, 2.143131898507868643E-15, -70.00000000000000000 ) ) ;
#4052 = CARTESIAN_POINT ( 'NONE',  ( 2.068961274655788607, 15.13167107497539376, -217.8084559455312501 ) ) ;
#4053 = CARTESIAN_POINT ( 'NONE',  ( 13.70635042947887428, -1.390919209824193592, -225.3477037409554953 ) ) ;
#4054 = CARTESIAN_POINT ( 'NONE',  ( 17.89221702206198117, 0.2742047965568425449, -220.2420650470893122 ) ) ;
#4055 = CARTESIAN_POINT ( 'NONE',  ( 14.31308345469695453, 12.76656023072872159, -231.9445021321040770 ) ) ;
#4056 = CIRCLE ( 'NONE', #2259, 2.000000000000000000 ) ;
#4057 = AXIS2_PLACEMENT_3D ( 'NONE', #21912, #8314, #3536 ) ;
#4058 = CARTESIAN_POINT ( 'NONE',  ( -22.19673167533144564, -9.562764463827019057, -233.1557790568585062 ) ) ;
#4059 = CARTESIAN_POINT ( 'NONE',  ( -9.060295054034883222, 29.20313342278041802, -224.2979742714222482 ) ) ;
#4060 = CARTESIAN_POINT ( 'NONE',  ( -0.8413160509385254615, -28.71376977722865931, -218.8117683208458288 ) ) ;
#4061 = CARTESIAN_POINT ( 'NONE',  ( 4.883314309504700468, 19.06839645569368358, -217.0171359871271193 ) ) ;
#4062 = CARTESIAN_POINT ( 'NONE',  ( 5.982199551433209805, -30.67818700677413091, -221.2919386232889849 ) ) ;
#4063 = CARTESIAN_POINT ( 'NONE',  ( 15.37450427861381286, -5.898921106289613847E-14, -228.0000000000000853 ) ) ;
#4064 = CARTESIAN_POINT ( 'NONE',  ( -11.35482716595652875, 11.86850131893102223, -220.6599844941370350 ) ) ;
#4065 = CARTESIAN_POINT ( 'NONE',  ( 0.000000000000000000, 23.00000000000000355, -75.00000000000000000 ) ) ;
#4066 = CARTESIAN_POINT ( 'NONE',  ( -18.30524310960561252, -4.731645231655051909, -231.4308113063693781 ) ) ;
#4067 = CARTESIAN_POINT ( 'NONE',  ( 6.402706778685327116, 14.41397785959879307, -226.0127495172349086 ) ) ;
#4068 = CARTESIAN_POINT ( 'NONE',  ( -17.39737143130126285, 7.531548707695031375, -232.0788227848755696 ) ) ;
#4069 = CARTESIAN_POINT ( 'NONE',  ( -16.99821283087967672, -0.5135051709387361552, -216.2173766440975555 ) ) ;
#4070 = CARTESIAN_POINT ( 'NONE',  ( -19.73058714482073128, -19.33240507441191625, -228.8766180877602494 ) ) ;
#4071 = CARTESIAN_POINT ( 'NONE',  ( 26.56239871811266440, 9.439457669498057868, -217.7226690415261885 ) ) ;
#4072 = AXIS2_PLACEMENT_3D ( 'NONE', #9335, #12708, #16635 ) ;
#4073 = CIRCLE ( 'NONE', #8401, 5.000000000000004441 ) ;
#4074 = FACE_OUTER_BOUND ( 'NONE', #10781, .T. ) ;
#4075 = CARTESIAN_POINT ( 'NONE',  ( -6.608244874605412100, -9.640126028631323507, -223.8427097396816805 ) ) ;
#4076 = CARTESIAN_POINT ( 'NONE',  ( 9.336393807558161839, 27.79372469574263960, -228.5913636680961361 ) ) ;
#4077 = CARTESIAN_POINT ( 'NONE',  ( 21.38922145650625239, 17.10616209967719215, -217.8354246241890451 ) ) ;
#4078 = CARTESIAN_POINT ( 'NONE',  ( -9.523248388595575875, 12.31121908620753125, -221.6288572946744182 ) ) ;
#4079 = CARTESIAN_POINT ( 'NONE',  ( -5.543543819386913540, 14.51457927969963713, -217.3847528063896846 ) ) ;
#4080 = CARTESIAN_POINT ( 'NONE',  ( 16.31458447723494132, 2.619382102851042671, -229.5862799001085364 ) ) ;
#4081 = CARTESIAN_POINT ( 'NONE',  ( 14.18740332497314149, -14.20295060558812672, -230.7262566610843351 ) ) ;
#4082 = CARTESIAN_POINT ( 'NONE',  ( 4.999282783285113219, -13.99249059192112021, -223.3817383379047214 ) ) ;
#4083 = VERTEX_POINT ( 'NONE', #12114 ) ;
#4084 = FACE_OUTER_BOUND ( 'NONE', #17806, .T. ) ;
#4085 = CARTESIAN_POINT ( 'NONE',  ( 15.05360126642391450, 1.481754003466396963, -222.9454997252120734 ) ) ;
#4086 = CARTESIAN_POINT ( 'NONE',  ( 23.36729170583618398, -5.500043712341283531, -232.1593072787115375 ) ) ;
#4087 = CARTESIAN_POINT ( 'NONE',  ( -18.75993824683981970, -9.028840681436806292, -217.1556094966459227 ) ) ;
#4088 = AXIS2_PLACEMENT_3D ( 'NONE', #16522, #1100, #13367 ) ;
#4089 = CARTESIAN_POINT ( 'NONE',  ( -0.1947256686167265494, -30.94043057420685727, -223.1178397439027492 ) ) ;
#4090 = CARTESIAN_POINT ( 'NONE',  ( 7.017641603801325623, 14.96204511409594673, -228.1064041248110073 ) ) ;
#4091 = CARTESIAN_POINT ( 'NONE',  ( 0.000000000000000000, 0.000000000000000000, 69.99999999999998579 ) ) ;
#4092 = CARTESIAN_POINT ( 'NONE',  ( -17.17143024911216287, 2.756036084795755681, -233.9491886983466316 ) ) ;
#4093 = TOROIDAL_SURFACE ( 'NONE', #2665, 24.63401512838761320, 3.000000000000035083 ) ;
#4094 = CARTESIAN_POINT ( 'NONE',  ( -10.24288955603410933, 28.30762631303078791, -220.8855665231519083 ) ) ;
#4095 = CARTESIAN_POINT ( 'NONE',  ( 1.455106383990497187, 21.12056149333958999, -230.8076663600630241 ) ) ;
#4096 = CARTESIAN_POINT ( 'NONE',  ( 13.49429091642815770, -0.3433647160923702368, -223.9641315955981895 ) ) ;
#4097 = CARTESIAN_POINT ( 'NONE',  ( 10.49811526528768368, 13.26166588535847701, -217.9009921269571919 ) ) ;
#4098 = CARTESIAN_POINT ( 'NONE',  ( -22.03660207690921879, 17.07234836129451949, -222.7335359861421296 ) ) ;
#4099 = CARTESIAN_POINT ( 'NONE',  ( 14.81251837262747983, -1.020578734748967209, -221.0290343291311785 ) ) ;
#4100 = CARTESIAN_POINT ( 'NONE',  ( 1.874647746501092893, -15.20125101474619633, -222.7462710229423521 ) ) ;
#4101 = DIRECTION ( 'NONE',  ( 1.000000000000000000, 0.000000000000000000, 0.000000000000000000 ) ) ;
#4102 = DIRECTION ( 'NONE',  ( -1.000000000000000000, 0.000000000000000000, 0.000000000000000000 ) ) ;
#4103 = CARTESIAN_POINT ( 'NONE',  ( 4.907833106823921376, 13.98151846258800290, -229.0190609869640923 ) ) ;
#4104 = CARTESIAN_POINT ( 'NONE',  ( -20.47121909278842722, -2.147015668718357695, -235.2226201655121258 ) ) ;
#4105 = CARTESIAN_POINT ( 'NONE',  ( -17.43458823433387650, 2.804998135793385750, -231.8077100320880959 ) ) ;
#4106 = CARTESIAN_POINT ( 'NONE',  ( 7.021536848793814123, -14.49751826649810482, -218.4909385705359455 ) ) ;
#4107 = SHAPE_DEFINITION_REPRESENTATION ( #79, #14642 ) ;
#4108 = CARTESIAN_POINT ( 'NONE',  ( 2.539761864897490007, 23.64215977235053501, -233.4645566207487661 ) ) ;
#4109 = AXIS2_PLACEMENT_3D ( 'NONE', #10961, #16243, #16035 ) ;
#4110 = CARTESIAN_POINT ( 'NONE',  ( -11.01414002179357610, 8.614420160880040811, -226.3770540798392972 ) ) ;
#4111 = ORIENTED_EDGE ( 'NONE', *, *, #13596, .T. ) ;
#4112 = CARTESIAN_POINT ( 'NONE',  ( -10.30050448363967419, 10.07750059423401190, -220.1837019037183723 ) ) ;
#4113 = CARTESIAN_POINT ( 'NONE',  ( -19.02606456345395358, -20.49905271945607055, -219.9673098173381902 ) ) ;
#4114 = DIRECTION ( 'NONE',  ( 0.000000000000000000, 0.000000000000000000, -1.000000000000000000 ) ) ;
#4115 = CARTESIAN_POINT ( 'NONE',  ( 25.50000000000000000, -3.600000000000001421, -2.699999999999999289 ) ) ;
#4116 = CARTESIAN_POINT ( 'NONE',  ( -4.104500432947460808, 15.73223271406093460, -218.0734292856946297 ) ) ;
#4117 = CARTESIAN_POINT ( 'NONE',  ( 3.881011284096109293, -13.04786028604701187, -224.6787317506201589 ) ) ;
#4118 = FILL_AREA_STYLE ('',( #3787 ) ) ;
#4119 = CARTESIAN_POINT ( 'NONE',  ( -13.56774755469388616, 7.311522441667196226, -219.1912666243428021 ) ) ;
#4120 = CARTESIAN_POINT ( 'NONE',  ( -31.04267853410473421, 7.029517189377418873, -226.8060334161593516 ) ) ;
#4121 = CARTESIAN_POINT ( 'NONE',  ( -1.565160934061885500, 18.19073094521525391, -232.0278805765578909 ) ) ;
#4122 = CARTESIAN_POINT ( 'NONE',  ( 1.665334536937735316E-13, -24.63401512838760610, 77.51594804401857175 ) ) ;
#4123 = CARTESIAN_POINT ( 'NONE',  ( 18.39384604806649648, 2.566915855367216004, -231.7421336352533103 ) ) ;
#4124 = CARTESIAN_POINT ( 'NONE',  ( -15.65248652229887405, -15.36320747609890169, -219.0899148657056230 ) ) ;
#4125 = B_SPLINE_CURVE_WITH_KNOTS ( 'NONE', 3,
 ( #12184, #21160, #259, #19474, #20944, #17696, #12294, #19038, #7011, #4063 ),
 .UNSPECIFIED., .F., .F.,
 ( 4, 2, 2, 2, 4 ),
 ( 0.003847469879456770925, 0.004275615195033988063, 0.004703760510611204766, 0.005131905826188422337, 0.005560051141765639041 ),
 .UNSPECIFIED. ) ;
#4126 = ORIENTED_EDGE ( 'NONE', *, *, #11026, .T. ) ;
#4127 = CARTESIAN_POINT ( 'NONE',  ( 7.213476267053916757, 16.78447451494783138, -217.5857052077849687 ) ) ;
#4128 = CARTESIAN_POINT ( 'NONE',  ( -7.266348978356541366, 16.38312187400933340, -217.9429203627011873 ) ) ;
#4129 = CARTESIAN_POINT ( 'NONE',  ( -8.308618357598591686, 12.44656112581930785, -228.0014162119141474 ) ) ;
#4130 = CARTESIAN_POINT ( 'NONE',  ( -18.95931133506032040, -20.40484553783743138, -225.1835090426186525 ) ) ;
#4131 = CARTESIAN_POINT ( 'NONE',  ( 0.000000000000000000, 0.000000000000000000, -24.99999999999999645 ) ) ;
#4132 = AXIS2_PLACEMENT_3D ( 'NONE', #7100, #230, #17449 ) ;
#4133 = VERTEX_POINT ( 'NONE', #3878 ) ;
#4134 =( GEOMETRIC_REPRESENTATION_CONTEXT ( 3 ) GLOBAL_UNCERTAINTY_ASSIGNED_CONTEXT ( ( #12593 ) ) GLOBAL_UNIT_ASSIGNED_CONTEXT ( ( #18657, #15061, #6726 ) ) REPRESENTATION_CONTEXT ( 'NONE', 'WORKASPACE' ) );
#4135 = CARTESIAN_POINT ( 'NONE',  ( -13.11494368899652052, 3.355507568391938200, -225.9121440085824304 ) ) ;
#4136 = CARTESIAN_POINT ( 'NONE',  ( -1.602612909676673469, -20.69807258397210248, -232.3153362903766492 ) ) ;
#4137 = CARTESIAN_POINT ( 'NONE',  ( 21.25094435758043332, 17.68230636442804027, -229.7964888993842010 ) ) ;
#4138 = CARTESIAN_POINT ( 'NONE',  ( 3.763426558366607111, 28.60172112197566818, -230.1816715025297526 ) ) ;
#4139 = EDGE_CURVE ( 'NONE', #21337, #16572, #10736, .T. ) ;
#4140 = CARTESIAN_POINT ( 'NONE',  ( -27.01279207917464475, 4.316569700791554887, -221.4451031230926219 ) ) ;
#4141 = CARTESIAN_POINT ( 'NONE',  ( 19.97628502126439187, 24.50819884991013708, -224.8824979922784735 ) ) ;
#4142 = CARTESIAN_POINT ( 'NONE',  ( 11.57669841200422134, 10.63052136557218574, -228.9489978335593889 ) ) ;
#4143 = CARTESIAN_POINT ( 'NONE',  ( 0.000000000000000000, 0.000000000000000000, 77.51594804401857175 ) ) ;
#4144 = CARTESIAN_POINT ( 'NONE',  ( -13.13432812001650341, -19.42279346457301514, -216.4126494286626610 ) ) ;
#4145 = CARTESIAN_POINT ( 'NONE',  ( 6.374306683232226156, -13.38367253400339330, -219.9651431149896723 ) ) ;
#4146 = CARTESIAN_POINT ( 'NONE',  ( 0.000000000000000000, 0.000000000000000000, 78.50000000000000000 ) ) ;
#4147 = DIRECTION ( 'NONE',  ( 0.000000000000000000, 0.000000000000000000, -1.000000000000000000 ) ) ;
#4148 = CARTESIAN_POINT ( 'NONE',  ( -4.591517861330576267, 12.55780501983563191, -223.5932882008353033 ) ) ;
#4149 = CARTESIAN_POINT ( 'NONE',  ( 18.01918173885548313, -1.728726289433203611, -215.5890043894241330 ) ) ;
#4150 = CARTESIAN_POINT ( 'NONE',  ( 20.80196158924851701, -7.261721507697286526, -217.3074963141844194 ) ) ;
#4151 = CARTESIAN_POINT ( 'NONE',  ( 10.49811526528768368, 13.26166588535847701, -217.9009921269571919 ) ) ;
#4152 = CARTESIAN_POINT ( 'NONE',  ( 10.90137817157632227, 16.64712710991609868, -230.5401786220292593 ) ) ;
#4153 = EDGE_LOOP ( 'NONE', ( #13725, #3352, #15634, #8574 ) ) ;
#4154 = CARTESIAN_POINT ( 'NONE',  ( 13.42370487565828796, -6.089723759188163221, -217.7532606872487406 ) ) ;
#4155 = CARTESIAN_POINT ( 'NONE',  ( 18.04365516558436866, 6.721233635139160612, -218.4376093631473168 ) ) ;
#4156 = CARTESIAN_POINT ( 'NONE',  ( 0.9169988354999972779, 20.59043933275470550, -235.2854195559275752 ) ) ;
#4157 = CARTESIAN_POINT ( 'NONE',  ( -5.028549462823471039, 18.55099042571767143, -234.6264744246184648 ) ) ;
#4158 = CARTESIAN_POINT ( 'NONE',  ( -23.30703516638871875, -0.6243632158918477337, -216.1214812734271220 ) ) ;
#4159 = CARTESIAN_POINT ( 'NONE',  ( -24.24202834850560606, 19.05981756344202438, -226.6980666352953335 ) ) ;
#4160 = CARTESIAN_POINT ( 'NONE',  ( 14.50000000000000000, 0.000000000000000000, 93.00000000000000000 ) ) ;
#4161 = EDGE_CURVE ( 'NONE', #5173, #161, #15697, .T. ) ;
#4162 = STYLED_ITEM ( 'NONE', ( #20832 ), #21952 ) ;
#4163 = CARTESIAN_POINT ( 'NONE',  ( 27.96460686140487084, -1.872811165202790340, -220.9791906660856000 ) ) ;
#4164 = CARTESIAN_POINT ( 'NONE',  ( -1.806671251568986669, 13.52068930966770388, -228.3567401718105430 ) ) ;
#4165 = CARTESIAN_POINT ( 'NONE',  ( 28.77543668145700195, 2.466904630248945907, -219.6646827587300947 ) ) ;
#4166 = CARTESIAN_POINT ( 'NONE',  ( -14.07917727715460821, 7.534853284453274291, -218.6337090155677458 ) ) ;
#4167 = CARTESIAN_POINT ( 'NONE',  ( 17.99029889091409018, 9.613712288440757092, -232.0298403238024036 ) ) ;
#4168 = CARTESIAN_POINT ( 'NONE',  ( 15.58734083230706524, 0.8631096974226073471, -227.8746545404512744 ) ) ;
#4169 = ADVANCED_FACE ( 'NONE', ( #20868 ), #14696, .T. ) ;
#4170 = EDGE_LOOP ( 'NONE', ( #21486, #15699, #13268, #3912 ) ) ;
#4171 = CARTESIAN_POINT ( 'NONE',  ( -1.837924626891132229, 29.27703531260187475, -227.2344808100871774 ) ) ;
#4172 = CARTESIAN_POINT ( 'NONE',  ( -13.72709560065558421, -5.132649126379569715, -227.9317987811764965 ) ) ;
#4173 = CARTESIAN_POINT ( 'NONE',  ( 5.343558017910363667, 26.29639771561252459, -218.1010331760174665 ) ) ;
#4174 = CARTESIAN_POINT ( 'NONE',  ( -7.753256282497156704, -15.05334625439219565, -219.2728364670455221 ) ) ;
#4175 = VECTOR ( 'NONE', #20468, 1000.000000000000000 ) ;
#4176 = LINE ( 'NONE', #10938, #19976 ) ;
#4177 = CARTESIAN_POINT ( 'NONE',  ( -13.31590776630363315, 5.340120742929252096, -225.6956515496373186 ) ) ;
#4178 = DIRECTION ( 'NONE',  ( 0.000000000000000000, 0.000000000000000000, 1.000000000000000000 ) ) ;
#4179 = CARTESIAN_POINT ( 'NONE',  ( 12.99512476935412231, -3.120572961704727977, -223.7636045402963987 ) ) ;
#4180 = CARTESIAN_POINT ( 'NONE',  ( 4.894897393135387631, 18.48819632322109996, -230.2131424875790628 ) ) ;
#4181 = CARTESIAN_POINT ( 'NONE',  ( -22.24722865165759345, 18.77558306771206986, -226.5077042908023941 ) ) ;
#4182 = CARTESIAN_POINT ( 'NONE',  ( -29.65068623107463708, 4.004319520977249525, -231.5200339834770773 ) ) ;
#4183 = CARTESIAN_POINT ( 'NONE',  ( -13.15060755141140980, -21.73659206351220519, -231.8601396556976226 ) ) ;
#4184 = CARTESIAN_POINT ( 'NONE',  ( 13.85207896949186335, 7.847214149978243292, -217.3457543576531066 ) ) ;
#4185 = CARTESIAN_POINT ( 'NONE',  ( -1.322875655532295358, 1.500000000000000000, -378.2244600276337678 ) ) ;
#4186 = CARTESIAN_POINT ( 'NONE',  ( -12.86575055733568540, -10.70886189207742589, -216.1397835820578450 ) ) ;
#4187 = CARTESIAN_POINT ( 'NONE',  ( -2.435715273212520238, 23.41098772907853132, -217.6796576669356966 ) ) ;
#4188 = CARTESIAN_POINT ( 'NONE',  ( 17.23498165643884761, 6.576565757823654934, -216.5785374982484655 ) ) ;
#4189 = CARTESIAN_POINT ( 'NONE',  ( -18.59263364681495290, 22.28600439725833482, -224.9897462721271779 ) ) ;
#4190 = CARTESIAN_POINT ( 'NONE',  ( 19.29971334243027314, 24.42889259816135095, -228.2141526116784291 ) ) ;
#4191 = ORIENTED_EDGE ( 'NONE', *, *, #2321, .F. ) ;
#4192 = CARTESIAN_POINT ( 'NONE',  ( -3.368184987477955694, -15.91886893360235078, -219.1066823976216256 ) ) ;
#4193 = CARTESIAN_POINT ( 'NONE',  ( 6.250374750423979719, -27.98416211894771521, -222.2453514702945085 ) ) ;
#4194 = DIRECTION ( 'NONE',  ( -1.000000000000000000, -1.224646799147353454E-16, 0.000000000000000000 ) ) ;
#4195 = CARTESIAN_POINT ( 'NONE',  ( 18.04365516558436866, 6.721233635139160612, -218.4376093631473168 ) ) ;
#4196 = CARTESIAN_POINT ( 'NONE',  ( 12.13827923251525220, -9.172799829723585319, -229.1860353116090891 ) ) ;
#4197 = CARTESIAN_POINT ( 'NONE',  ( -17.42499862437977853, -18.98713029041037004, -232.7811807006768845 ) ) ;
#4198 = CARTESIAN_POINT ( 'NONE',  ( -19.50907964299920039, -17.77536300509877876, -217.8007844881196320 ) ) ;
#4199 = CARTESIAN_POINT ( 'NONE',  ( 3.388180927852674884, 15.71154068801650538, -224.9339660840813053 ) ) ;
#4200 = DIRECTION ( 'NONE',  ( 0.000000000000000000, 0.000000000000000000, -1.000000000000000000 ) ) ;
#4201 = CARTESIAN_POINT ( 'NONE',  ( 14.32363442937021425, 2.978337679677412808, -227.0386046113487453 ) ) ;
#4202 = CARTESIAN_POINT ( 'NONE',  ( -3.501680520304516264, 14.31538576447642264, -219.8967178229432307 ) ) ;
#4203 = CARTESIAN_POINT ( 'NONE',  ( -3.130917144532865848, 26.01013079854885390, -229.4331404728494874 ) ) ;
#4204 = CARTESIAN_POINT ( 'NONE',  ( 29.83024462204712179, 0.7507192471929857724, -227.4186229137179396 ) ) ;
#4205 = ORIENTED_EDGE ( 'NONE', *, *, #11174, .F. ) ;
#4206 = CARTESIAN_POINT ( 'NONE',  ( 11.64932556965463561, 7.668732705389711413, -229.0406978839571366 ) ) ;
#4207 = CARTESIAN_POINT ( 'NONE',  ( -14.59766675578715223, 7.926254675926275972, -222.3706877972550444 ) ) ;
#4208 = CARTESIAN_POINT ( 'NONE',  ( 19.49137065790598555, 9.165486118354671419, -234.8706749352814995 ) ) ;
#4209 = CARTESIAN_POINT ( 'NONE',  ( 0.7797512750231831991, -26.58197935702783354, -230.4407411870234625 ) ) ;
#4210 = FACE_BOUND ( 'NONE', #14141, .T. ) ;
#4211 = VERTEX_POINT ( 'NONE', #3548 ) ;
#4212 = CARTESIAN_POINT ( 'NONE',  ( 12.04687593227112430, 27.54339840196571743, -224.6466266724203820 ) ) ;
#4213 = CARTESIAN_POINT ( 'NONE',  ( 22.59847068942421444, -14.29990159211854106, -221.3422834976353499 ) ) ;
#4214 = CARTESIAN_POINT ( 'NONE',  ( 0.000000000000000000, 0.000000000000000000, 75.34729635533385306 ) ) ;
#4215 = CARTESIAN_POINT ( 'NONE',  ( -6.722478243781921492, -14.20656108661463612, -231.4169491518476889 ) ) ;
#4216 = CARTESIAN_POINT ( 'NONE',  ( 0.7245137624042983227, 13.44764381486384330, -223.4043886706536455 ) ) ;
#4217 = CARTESIAN_POINT ( 'NONE',  ( -5.373457274256926652, 30.83572167890261184, -229.2199105909169532 ) ) ;
#4218 = ORIENTED_EDGE ( 'NONE', *, *, #14942, .T. ) ;
#4219 = CARTESIAN_POINT ( 'NONE',  ( -9.250876228778270871, 9.538614635316015722, -227.1332118982684563 ) ) ;
#4220 = CARTESIAN_POINT ( 'NONE',  ( -20.63475909113443763, -3.483688486440585486, -233.7225001494461480 ) ) ;
#4221 = CARTESIAN_POINT ( 'NONE',  ( 0.000000000000000000, 0.000000000000000000, -78.50000000000000000 ) ) ;
#4222 = CARTESIAN_POINT ( 'NONE',  ( -22.99261559126758314, 0.6704778918838653068, -9.983049392048402026 ) ) ;
#4223 = EDGE_CURVE ( 'NONE', #13811, #1604, #10759, .T. ) ;
#4224 = CARTESIAN_POINT ( 'NONE',  ( -9.443239614166923701, 9.388015667058336788, -222.3195230688234290 ) ) ;
#4225 = CARTESIAN_POINT ( 'NONE',  ( 8.990474075060864934, -28.03008174514034678, -221.5310560963409330 ) ) ;
#4226 = CARTESIAN_POINT ( 'NONE',  ( 24.59129902578158067, -8.191391589517788674, -218.4338547727923299 ) ) ;
#4227 = CARTESIAN_POINT ( 'NONE',  ( -25.80904414196669450, 12.19501778665756220, -219.1732313092283846 ) ) ;
#4228 = CARTESIAN_POINT ( 'NONE',  ( 15.80790828609669951, 3.698719088746416972, -219.8106174092292804 ) ) ;
#4229 = CARTESIAN_POINT ( 'NONE',  ( -7.834600152078401436, 27.83486203824852012, -220.1209588485844222 ) ) ;
#4230 = CARTESIAN_POINT ( 'NONE',  ( 13.75457993763798648, 0.05083669377823854529, -228.0000000000000853 ) ) ;
#4231 = CARTESIAN_POINT ( 'NONE',  ( 17.32394486779715592, 4.028159306070694612, -218.4253989884176690 ) ) ;
#4232 = CARTESIAN_POINT ( 'NONE',  ( -11.18644257538908526, -20.90776414258732174, -230.8249452324125173 ) ) ;
#4233 = ORIENTED_EDGE ( 'NONE', *, *, #2395, .T. ) ;
#4234 = CARTESIAN_POINT ( 'NONE',  ( 9.527502190795640757, 23.55559004943647139, -217.4101659741468211 ) ) ;
#4235 = CARTESIAN_POINT ( 'NONE',  ( -11.13829636790841704, 14.30978168460582189, -218.6922574227322400 ) ) ;
#4236 = CARTESIAN_POINT ( 'NONE',  ( -12.33997807949817904, 15.01940705987184188, -217.6798968600957380 ) ) ;
#4237 = CARTESIAN_POINT ( 'NONE',  ( 23.84888352507021736, -3.411310983279423947, -216.3556234003997645 ) ) ;
#4238 = DIRECTION ( 'NONE',  ( -1.000000000000000000, 0.000000000000000000, 0.000000000000000000 ) ) ;
#4239 = ORIENTED_EDGE ( 'NONE', *, *, #22215, .F. ) ;
#4240 = CARTESIAN_POINT ( 'NONE',  ( 18.79638869589749461, 0.4878066561304963966, -219.5712168927955759 ) ) ;
#4241 = CARTESIAN_POINT ( 'NONE',  ( -5.474373895759362618, -29.29005893717160092, -223.2371403555430334 ) ) ;
#4242 = CARTESIAN_POINT ( 'NONE',  ( 15.15867943830037134, 1.437942759855808772, -227.6349539663164876 ) ) ;
#4243 = CARTESIAN_POINT ( 'NONE',  ( 4.340445191644851874, 29.86837761166362881, -227.4879512554873315 ) ) ;
#4244 = CARTESIAN_POINT ( 'NONE',  ( 14.87215633904093082, -2.419155424398304888, -226.7769793042785125 ) ) ;
#4245 = CARTESIAN_POINT ( 'NONE',  ( -25.06333669508177309, 2.553070212212491530, -230.2963116797556893 ) ) ;
#4246 = CARTESIAN_POINT ( 'NONE',  ( 23.83082175545800752, 15.77842900014857896, -219.5351905769044834 ) ) ;
#4247 = EDGE_CURVE ( 'NONE', #20174, #17900, #5341, .T. ) ;
#4248 = CARTESIAN_POINT ( 'NONE',  ( 21.35706335192880445, 15.67286272432725092, -219.2578158352350783 ) ) ;
#4249 = AXIS2_PLACEMENT_3D ( 'NONE', #17517, #15827, #184 ) ;
#4250 = CYLINDRICAL_SURFACE ( 'NONE', #8056, 3.000000000000002665 ) ;
#4251 = CARTESIAN_POINT ( 'NONE',  ( -26.69331514234889013, -17.84497232456928373, -223.5918739730229845 ) ) ;
#4252 = CARTESIAN_POINT ( 'NONE',  ( -20.11874861854083463, -21.11755179634840474, -229.7504124090357323 ) ) ;
#4253 = CARTESIAN_POINT ( 'NONE',  ( 5.451525948382545117, -12.45300865616632713, -227.8545162512558306 ) ) ;
#4254 = CARTESIAN_POINT ( 'NONE',  ( -21.59054411123144135, -7.930690890291152151, -6.099882278136012026 ) ) ;
#4255 = CARTESIAN_POINT ( 'NONE',  ( 0.000000000000000000, -23.00000000000000000, -55.00000000000000000 ) ) ;
#4256 = CARTESIAN_POINT ( 'NONE',  ( -16.23478446547628096, 26.31175924651574149, -222.4178907105033431 ) ) ;
#4257 = CARTESIAN_POINT ( 'NONE',  ( 24.13177372007769961, -1.862525787088729956, -215.1116454360890202 ) ) ;
#4258 = CARTESIAN_POINT ( 'NONE',  ( 25.69761320619099720, -8.403105518750903613, -219.2599777650661110 ) ) ;
#4259 = CARTESIAN_POINT ( 'NONE',  ( -26.38808873681881906, 13.30696350521622939, -225.1492950792419663 ) ) ;
#4260 = CARTESIAN_POINT ( 'NONE',  ( 18.23116248274160256, 13.99874872632082123, -216.0593560670294835 ) ) ;
#4261 = CARTESIAN_POINT ( 'NONE',  ( 12.60818910183731489, 13.02403301690871729, -229.3305689548085695 ) ) ;
#4262 = ORIENTED_EDGE ( 'NONE', *, *, #3598, .F. ) ;
#4263 = CARTESIAN_POINT ( 'NONE',  ( 5.517988016436452980, -29.70724229459007759, -226.4438119151823514 ) ) ;
#4264 = FACE_OUTER_BOUND ( 'NONE', #16799, .T. ) ;
#4265 = CARTESIAN_POINT ( 'NONE',  ( -8.123851230256436295, 20.56863949923577550, -215.0796075421103239 ) ) ;
#4266 = CARTESIAN_POINT ( 'NONE',  ( -12.80532875684362715, 24.61139456694233374, -232.5885756414849084 ) ) ;
#4267 = CARTESIAN_POINT ( 'NONE',  ( -16.38803511840525218, -9.809678413005567421, -217.1940421839195494 ) ) ;
#4268 = CARTESIAN_POINT ( 'NONE',  ( -15.66530208164916260, 23.23467148471576849, -218.1250122661128046 ) ) ;
#4269 = CARTESIAN_POINT ( 'NONE',  ( -14.50000000000000000, 1.775737858763662015E-15, 93.00000000000000000 ) ) ;
#4270 = CARTESIAN_POINT ( 'NONE',  ( 29.12543877365354916, -1.475122899492763873, -224.0746120762670444 ) ) ;
#4271 = CARTESIAN_POINT ( 'NONE',  ( -4.651113456395510326, 27.58151660986499110, -218.3072938287727141 ) ) ;
#4272 = CARTESIAN_POINT ( 'NONE',  ( -16.08005950484750102, -0.1764640578214327904, -223.5999988222837942 ) ) ;
#4273 = CARTESIAN_POINT ( 'NONE',  ( -16.65698539163286540, 11.03290537638306112, -233.6474915129378758 ) ) ;
#4274 = CARTESIAN_POINT ( 'NONE',  ( 17.00168025137501004, 6.212099629982537508, -219.0548246536471595 ) ) ;
#4275 = DIRECTION ( 'NONE',  ( -1.000000000000000000, 0.000000000000000000, 0.000000000000000000 ) ) ;
#4276 = CARTESIAN_POINT ( 'NONE',  ( 5.064106757301036765, 16.06517852189101703, -221.6413221086847329 ) ) ;
#4277 = CARTESIAN_POINT ( 'NONE',  ( -24.15031621174628285, -13.05338392360020627, -219.0842748323915714 ) ) ;
#4278 = CARTESIAN_POINT ( 'NONE',  ( 15.87442104186276381, 8.674488492264579520, -230.9702037640878416 ) ) ;
#4279 = CARTESIAN_POINT ( 'NONE',  ( 1.040523496405688642, -16.53460264249922318, -217.0944950338946455 ) ) ;
#4280 = DIRECTION ( 'NONE',  ( -0.000000000000000000, -0.000000000000000000, -1.000000000000000000 ) ) ;
#4281 = ADVANCED_FACE ( 'NONE', ( #3650 ), #17199, .F. ) ;
#4282 = CARTESIAN_POINT ( 'NONE',  ( -13.96147744945181124, 5.260363697127891314, -222.3342733685200301 ) ) ;
#4283 = CARTESIAN_POINT ( 'NONE',  ( 15.56514059923893178, -9.210181625211102840, -232.5361143517874325 ) ) ;
#4284 = CARTESIAN_POINT ( 'NONE',  ( 15.03112630398312177, 24.11065413595933293, -226.8236212149936080 ) ) ;
#4285 = CARTESIAN_POINT ( 'NONE',  ( -24.39036648059286350, 13.21953970265592027, -220.1632778389106591 ) ) ;
#4286 = CARTESIAN_POINT ( 'NONE',  ( -16.81617677814535128, 0.6259372974186930838, -233.5115673467681745 ) ) ;
#4287 = CARTESIAN_POINT ( 'NONE',  ( -22.88587990158785601, -12.52061884883742238, -220.5813279352508687 ) ) ;
#4288 = CARTESIAN_POINT ( 'NONE',  ( 11.75404126451729070, 5.688294280104953415, -229.3533586468489602 ) ) ;
#4289 = FACE_OUTER_BOUND ( 'NONE', #18231, .T. ) ;
#4290 = CARTESIAN_POINT ( 'NONE',  ( -11.72787654052445028, -3.882995534642332824, -226.9210218758430244 ) ) ;
#4291 = CARTESIAN_POINT ( 'NONE',  ( 2.951582164238582440, 19.39026647431845873, -217.4356918981242472 ) ) ;
#4292 = CARTESIAN_POINT ( 'NONE',  ( -16.98287383830707142, 1.584866439881522648, -221.5391863673846444 ) ) ;
#4293 = CARTESIAN_POINT ( 'NONE',  ( -5.629016366058284149, 14.31889596247328633, -229.4177297515988414 ) ) ;
#4294 = CARTESIAN_POINT ( 'NONE',  ( 11.84598249547323690, 10.36127485500543699, -218.5481300776139904 ) ) ;
#4295 = CARTESIAN_POINT ( 'NONE',  ( -4.782174899302804150, -29.09898918907212817, -227.3916599557566940 ) ) ;
#4296 = CARTESIAN_POINT ( 'NONE',  ( -1.339836966046043631, -21.49735173129188581, -217.9043760890963313 ) ) ;
#4297 = CARTESIAN_POINT ( 'NONE',  ( 16.91879448796214191, 0.8271603773820436212, -230.0510230802265710 ) ) ;
#4298 = CARTESIAN_POINT ( 'NONE',  ( 11.78320976064766690, -8.193118641535518165, -222.2581747538435479 ) ) ;
#4299 = CARTESIAN_POINT ( 'NONE',  ( 16.22685372911609036, -0.3790667790403521309, -218.4894315352551644 ) ) ;
#4300 = CARTESIAN_POINT ( 'NONE',  ( -5.525229149912007642, -13.32411127922494742, -220.4018445532201440 ) ) ;
#4301 = CARTESIAN_POINT ( 'NONE',  ( 15.50648685944955218, 24.16641006378193168, -224.4827813270165393 ) ) ;
#4302 = LINE ( 'NONE', #4747, #15666 ) ;
#4303 = CARTESIAN_POINT ( 'NONE',  ( -24.69837543585720141, 12.57569301576483589, -232.4521327773205428 ) ) ;
#4304 = CARTESIAN_POINT ( 'NONE',  ( 4.389496648589924277, 14.47660514356954131, -220.6151178996808540 ) ) ;
#4305 = CARTESIAN_POINT ( 'NONE',  ( 4.894897393135387631, 18.48819632322109996, -230.2131424875790628 ) ) ;
#4306 = CARTESIAN_POINT ( 'NONE',  ( 29.31647908907816102, 0.9594737942742700421, -228.5782466420670858 ) ) ;
#4307 = ORIENTED_EDGE ( 'NONE', *, *, #10113, .F. ) ;
#4308 = CARTESIAN_POINT ( 'NONE',  ( 16.64575860537911112, 25.12688477742292648, -227.5050599151411745 ) ) ;
#4309 = CARTESIAN_POINT ( 'NONE',  ( -13.58070052954164275, 11.19572749768420650, -220.2511552028196604 ) ) ;
#4310 = CARTESIAN_POINT ( 'NONE',  ( -25.94982248293519689, 10.67899231259548287, -221.1273147719203962 ) ) ;
#4311 = CARTESIAN_POINT ( 'NONE',  ( 5.191785474240024456, -25.78595846473334419, -219.2330600099714673 ) ) ;
#4312 = CARTESIAN_POINT ( 'NONE',  ( 0.000000000000000000, 0.000000000000000000, -60.00000000000001421 ) ) ;
#4313 = DIRECTION ( 'NONE',  ( 0.000000000000000000, 0.000000000000000000, 1.000000000000000000 ) ) ;
#4314 = CARTESIAN_POINT ( 'NONE',  ( 5.169766346882679997, 29.28517558595074988, -221.5178724947562614 ) ) ;
#4315 = CARTESIAN_POINT ( 'NONE',  ( 12.91525526572063853, -9.549346049255611035, -226.1928206613168584 ) ) ;
#4316 = DIRECTION ( 'NONE',  ( -1.000000000000000000, 0.000000000000000000, 0.000000000000000000 ) ) ;
#4317 = EDGE_CURVE ( 'NONE', #18628, #1930, #10534, .T. ) ;
#4318 = CARTESIAN_POINT ( 'NONE',  ( -7.832594822155400927, -23.57318293858060088, -216.4298491688572028 ) ) ;
#4319 = CARTESIAN_POINT ( 'NONE',  ( -3.755296588130283553, 23.77975947300719284, -233.7323173085780752 ) ) ;
#4320 = CARTESIAN_POINT ( 'NONE',  ( -0.04850409037381671340, 14.20520396026658716, -231.8092226852533031 ) ) ;
#4321 = VERTEX_POINT ( 'NONE', #2521 ) ;
#4322 = CARTESIAN_POINT ( 'NONE',  ( -18.47334320050258327, 24.79293862780133040, -226.9986786077537317 ) ) ;
#4323 = CARTESIAN_POINT ( 'NONE',  ( -25.34460520202507539, -7.988444519707189606, -217.6292756219348234 ) ) ;
#4324 = CARTESIAN_POINT ( 'NONE',  ( -22.91992063051224449, -9.983913345421759900, 0.6574913861358061551 ) ) ;
#4325 = FACE_BOUND ( 'NONE', #5598, .T. ) ;
#4326 = CARTESIAN_POINT ( 'NONE',  ( -11.02345917017863464, 29.02019856777526741, -223.9475008740665771 ) ) ;
#4327 = CARTESIAN_POINT ( 'NONE',  ( -6.183400735100206269, -24.17720054222102277, -215.4627583112813625 ) ) ;
#4328 = CARTESIAN_POINT ( 'NONE',  ( 0.000000000000000000, 0.000000000000000000, 77.51594804401857175 ) ) ;
#4329 = CARTESIAN_POINT ( 'NONE',  ( -12.44873260470819787, 7.411970124596155785, -229.4214091473984070 ) ) ;
#4330 = CARTESIAN_POINT ( 'NONE',  ( -11.78887577478644566, 1.715692547334320084, -224.3106172711415525 ) ) ;
#4331 = CARTESIAN_POINT ( 'NONE',  ( 0.9879969248128627202, 20.02408072508558945, -218.2055348255049410 ) ) ;
#4332 = FACE_OUTER_BOUND ( 'NONE', #8944, .T. ) ;
#4333 = CARTESIAN_POINT ( 'NONE',  ( 23.24653631066306048, 11.83805845626388020, -219.6020901153134162 ) ) ;
#4334 = CARTESIAN_POINT ( 'NONE',  ( -12.75670220164522384, -23.12103459569904373, -229.1084755445707799 ) ) ;
#4335 = ORIENTED_EDGE ( 'NONE', *, *, #7895, .F. ) ;
#4336 = CARTESIAN_POINT ( 'NONE',  ( 10.25948093768852054, 28.38842464930171872, -224.3436940787075855 ) ) ;
#4337 = CARTESIAN_POINT ( 'NONE',  ( 1.833772325875588027, 13.50593961039006707, -219.8748197804281119 ) ) ;
#4338 = CARTESIAN_POINT ( 'NONE',  ( -9.734169867326336600, 14.53420431798807755, -231.2442251076483046 ) ) ;
#4339 = CARTESIAN_POINT ( 'NONE',  ( -16.02921639098982709, -5.689335215210093999, -220.0011032104688979 ) ) ;
#4340 = CARTESIAN_POINT ( 'NONE',  ( 25.00000000000001066, -3.061616997868384226E-15, -75.00000000000000000 ) ) ;
#4341 = ORIENTED_EDGE ( 'NONE', *, *, #14266, .F. ) ;
#4342 = CARTESIAN_POINT ( 'NONE',  ( -16.63766460830045091, 5.158675778507696208, -232.1659425527909093 ) ) ;
#4343 = CARTESIAN_POINT ( 'NONE',  ( -13.40300228573463848, -19.05792172404923690, -234.2100255530988306 ) ) ;
#4344 = CARTESIAN_POINT ( 'NONE',  ( 22.18132842682159733, 5.591149267797686839, -232.0584733989884114 ) ) ;
#4345 = CARTESIAN_POINT ( 'NONE',  ( 4.343013938751969505, 13.02036404005131587, -224.7825435359082178 ) ) ;
#4346 = CARTESIAN_POINT ( 'NONE',  ( 0.000000000000000000, 24.63401512838747820, 77.51594804401857175 ) ) ;
#4347 = CARTESIAN_POINT ( 'NONE',  ( -16.66929017373293931, 3.065794289431343689, -220.7800282905443794 ) ) ;
#4348 = CARTESIAN_POINT ( 'NONE',  ( 9.253342549662157523, 15.33540844142859605, -216.2601104504267937 ) ) ;
#4349 = CARTESIAN_POINT ( 'NONE',  ( -23.13858343966594688, 9.466612565523535139, -3.238977037839615214 ) ) ;
#4350 = CARTESIAN_POINT ( 'NONE',  ( 22.86997486125673618, 17.56009411325475966, -222.3578648042903296 ) ) ;
#4351 = DIRECTION ( 'NONE',  ( -1.000000000000000000, 0.000000000000000000, 0.000000000000000000 ) ) ;
#4352 = CARTESIAN_POINT ( 'NONE',  ( 24.96598054343045447, -3.653363829669123319, -219.8248103142179559 ) ) ;
#4353 = CARTESIAN_POINT ( 'NONE',  ( -19.31342342724724759, -3.870051895940637365, -217.8584481481169348 ) ) ;
#4354 = CARTESIAN_POINT ( 'NONE',  ( 0.000000000000000000, 0.000000000000000000, -70.00000000000000000 ) ) ;
#4355 = PRODUCT_RELATED_PRODUCT_CATEGORY ( 'part', '', ( #10136 ) ) ;
#4356 = VECTOR ( 'NONE', #12727, 1000.000000000000000 ) ;
#4357 = DIRECTION ( 'NONE',  ( -0.000000000000000000, -0.000000000000000000, -1.000000000000000000 ) ) ;
#4358 = CARTESIAN_POINT ( 'NONE',  ( -8.201407585998298444, 17.38801480109368924, -216.6295241303755006 ) ) ;
#4359 = CARTESIAN_POINT ( 'NONE',  ( 15.13468687495441323, -1.603572186776826447, -217.3101985623318626 ) ) ;
#4360 = CARTESIAN_POINT ( 'NONE',  ( 14.64930099072384095, -2.233284345536625803, -226.6630761355773984 ) ) ;
#4361 = CARTESIAN_POINT ( 'NONE',  ( -25.64868633208605786, 12.30364128039660798, -229.0020209687957049 ) ) ;
#4362 = CARTESIAN_POINT ( 'NONE',  ( 9.211411085256067111, 16.86455563410128633, -232.8411836211112700 ) ) ;
#4363 = CARTESIAN_POINT ( 'NONE',  ( 20.90058474538433231, 18.60939544422136294, -225.8027644507526475 ) ) ;
#4364 = ORIENTED_EDGE ( 'NONE', *, *, #8228, .T. ) ;
#4365 = CARTESIAN_POINT ( 'NONE',  ( 3.303203443418958773, -15.45560242990989686, -230.9065799468681917 ) ) ;
#4366 = CARTESIAN_POINT ( 'NONE',  ( 11.41432417523484055, 8.992600385930652251, 93.00000000000000000 ) ) ;
#4367 = CIRCLE ( 'NONE', #16969, 3.000000000000002665 ) ;
#4368 = CARTESIAN_POINT ( 'NONE',  ( 4.213939275857851108, 16.79797086795582928, -215.8378124706958943 ) ) ;
#4369 = CARTESIAN_POINT ( 'NONE',  ( -4.424820997438546399, 11.84746159238278373, -221.7815792475208525 ) ) ;
#4370 = CARTESIAN_POINT ( 'NONE',  ( 15.03150297321239925, -8.313127316319620874, -220.7815108570360394 ) ) ;
#4371 = CARTESIAN_POINT ( 'NONE',  ( -0.9414827276148034496, 23.96885519606619752, -216.4491898092606164 ) ) ;
#4372 = CARTESIAN_POINT ( 'NONE',  ( -10.42709000561872834, -10.07820250684338603, 93.00000000000001421 ) ) ;
#4373 = AXIS2_PLACEMENT_3D ( 'NONE', #14970, #4701, #14853 ) ;
#4374 = CARTESIAN_POINT ( 'NONE',  ( 2.631948090663005946, 31.21493676147814611, -222.3107766067421380 ) ) ;
#4375 = CARTESIAN_POINT ( 'NONE',  ( -15.94549496081242346, -0.04271059606100771622, -224.7066567765017169 ) ) ;
#4376 = CARTESIAN_POINT ( 'NONE',  ( -11.24282496690421596, 12.44430180464951086, -232.4405891940542404 ) ) ;
#4377 = CARTESIAN_POINT ( 'NONE',  ( 20.89184612657454920, 5.404957034965973683, -232.0952743654565609 ) ) ;
#4378 = CARTESIAN_POINT ( 'NONE',  ( 3.673290835002071653, 15.92545533070904895, -226.4848186297188022 ) ) ;
#4379 = DIRECTION ( 'NONE',  ( 1.083936797661035110E-15, 1.000000000000000000, 0.000000000000000000 ) ) ;
#4380 = ORIENTED_EDGE ( 'NONE', *, *, #12449, .F. ) ;
#4381 = CARTESIAN_POINT ( 'NONE',  ( -1.696080206444520844, 14.74162257415073540, -222.2455536759108838 ) ) ;
#4382 = CARTESIAN_POINT ( 'NONE',  ( -18.64257584594551531, -16.66392856591270899, -217.1407738418131999 ) ) ;
#4383 = CARTESIAN_POINT ( 'NONE',  ( 14.73698509926073186, 4.443590625350892331, -227.4062002049096236 ) ) ;
#4384 = CARTESIAN_POINT ( 'NONE',  ( -9.870642741937645681, -28.68889699630894441, -223.8025096038410879 ) ) ;
#4385 = DIRECTION ( 'NONE',  ( -0.000000000000000000, -0.000000000000000000, 1.000000000000000000 ) ) ;
#4386 = CIRCLE ( 'NONE', #13033, 23.00000000000008882 ) ;
#4387 = CARTESIAN_POINT ( 'NONE',  ( -22.04240660558204823, 19.10355008918698871, -223.9524535985323723 ) ) ;
#4388 = CARTESIAN_POINT ( 'NONE',  ( 23.27685575300125720, -16.81362096763192326, -220.1650456318757563 ) ) ;
#4389 = CARTESIAN_POINT ( 'NONE',  ( 6.225744896574323839, 14.38227537199079720, -224.8391693295998266 ) ) ;
#4390 = CARTESIAN_POINT ( 'NONE',  ( -13.75208518020500748, 5.661250135068270239, -227.6647651141479685 ) ) ;
#4391 = CARTESIAN_POINT ( 'NONE',  ( -11.10543627608095285, 3.497967533612860613, -224.1342318769322617 ) ) ;
#4392 = CARTESIAN_POINT ( 'NONE',  ( -13.72723917162997154, -9.146515947596070006, -227.8820830806802746 ) ) ;
#4393 = B_SPLINE_CURVE_WITH_KNOTS ( 'NONE', 3,
 ( #19986, #871, #11449, #4242, #21340, #18317, #19657, #5935, #17990, #2552, #6043, #2877, #16624, #9436, #16296, #7750, #14620, #21454 ),
 .UNSPECIFIED., .F., .F.,
 ( 4, 2, 2, 2, 2, 2, 2, 2, 4 ),
 ( 2.482325801946720893E-17, 0.0004266872910318495827, 0.0008533745820636743371, 0.001280061873095498983, 0.001706749164127323738, 0.002133436455159148492, 0.002560123746190973246, 0.002986811037222798001, 0.003413498328254622755 ),
 .UNSPECIFIED. ) ;
#4394 = CARTESIAN_POINT ( 'NONE',  ( 14.81258087342262364, 2.398747990731791013, -230.9000679928271040 ) ) ;
#4395 = DIRECTION ( 'NONE',  ( 1.000000000000000000, 0.000000000000000000, 0.000000000000000000 ) ) ;
#4396 = CARTESIAN_POINT ( 'NONE',  ( -9.864471611369220128, -7.448779108659549841, -221.8449511945744064 ) ) ;
#4397 = CARTESIAN_POINT ( 'NONE',  ( 4.303123380281038024, 17.66787810618728827, -231.9745698734655832 ) ) ;
#4398 = CIRCLE ( 'NONE', #17007, 17.50000000000001066 ) ;
#4399 = CARTESIAN_POINT ( 'NONE',  ( 22.42925200799500729, 5.652256920629083581, -234.0734181799116698 ) ) ;
#4400 = EDGE_CURVE ( 'NONE', #19675, #6063, #15779, .T. ) ;
#4401 = CIRCLE ( 'NONE', #17353, 3.000000000000002665 ) ;
#4402 = CARTESIAN_POINT ( 'NONE',  ( -11.86888352782322897, 15.29489941890347282, -218.1379771575364259 ) ) ;
#4403 = CARTESIAN_POINT ( 'NONE',  ( 3.490829917597003895, 11.40812925993816229, -222.8973702487053004 ) ) ;
#4404 = ORIENTED_EDGE ( 'NONE', *, *, #15523, .T. ) ;
#4405 = CARTESIAN_POINT ( 'NONE',  ( 0.6532050297617689738, -21.40793743009686878, -217.7635283671393722 ) ) ;
#4406 = CARTESIAN_POINT ( 'NONE',  ( 0.4703770282364683197, -28.19050476347214484, -228.5103440588500519 ) ) ;
#4407 = CARTESIAN_POINT ( 'NONE',  ( 14.73698509926073186, 4.443590625350892331, -227.4062002049096236 ) ) ;
#4408 = CARTESIAN_POINT ( 'NONE',  ( 14.68556740487494849, -6.365102927765655672, -229.6664356779805587 ) ) ;
#4409 = CARTESIAN_POINT ( 'NONE',  ( -29.22168435891936156, -1.352755938724206519, -225.9547066689444250 ) ) ;
#4410 = CARTESIAN_POINT ( 'NONE',  ( -5.279374154171231126, -12.28263746854076466, -222.5283095625445640 ) ) ;
#4411 = CARTESIAN_POINT ( 'NONE',  ( 14.02816775221371337, 20.58276248714641810, -218.7180790146936999 ) ) ;
#4412 = FILL_AREA_STYLE ('',( #16363 ) ) ;
#4413 = CARTESIAN_POINT ( 'NONE',  ( 14.65309016725241698, 3.424799466898550637, -221.5217808432381048 ) ) ;
#4414 = CARTESIAN_POINT ( 'NONE',  ( 5.169766346882679997, 29.28517558595074988, -221.5178724947562614 ) ) ;
#4415 = CARTESIAN_POINT ( 'NONE',  ( -1.158668551263366986, 23.31492692626720853, -219.2372600964201865 ) ) ;
#4416 = CARTESIAN_POINT ( 'NONE',  ( 7.144703960786618957, -9.913249271193393497, -228.5244988832443198 ) ) ;
#4417 = AXIS2_PLACEMENT_3D ( 'NONE', #9597, #20139, #12966 ) ;
#4418 = CIRCLE ( 'NONE', #831, 3.000000000000002665 ) ;
#4419 = CARTESIAN_POINT ( 'NONE',  ( 9.798337081649805214, 12.27506320122302697, -218.9346733583377613 ) ) ;
#4420 = CARTESIAN_POINT ( 'NONE',  ( -20.29166677327761903, 16.18344358422343632, -220.0060062064338524 ) ) ;
#4421 = CARTESIAN_POINT ( 'NONE',  ( -18.04102731735134313, 0.8647102676311391178, -229.4625228093430849 ) ) ;
#4422 = CARTESIAN_POINT ( 'NONE',  ( 1.632321987819951969, -14.78074153629778387, -224.5834756332612301 ) ) ;
#4423 = CARTESIAN_POINT ( 'NONE',  ( 0.000000000000000000, 0.000000000000000000, -70.00000000000000000 ) ) ;
#4424 = DIRECTION ( 'NONE',  ( 0.000000000000000000, 0.000000000000000000, 1.000000000000000000 ) ) ;
#4425 = CARTESIAN_POINT ( 'NONE',  ( 26.29894631880581812, 12.29609390142961090, -226.3100047295820332 ) ) ;
#4426 = CARTESIAN_POINT ( 'NONE',  ( 10.81635663018848525, -11.46278932037511566, -222.6527676248099681 ) ) ;
#4427 = DIRECTION ( 'NONE',  ( 0.000000000000000000, 0.000000000000000000, -1.000000000000000000 ) ) ;
#4428 = EDGE_CURVE ( 'NONE', #22217, #19675, #9512, .T. ) ;
#4429 = CARTESIAN_POINT ( 'NONE',  ( -5.636842872076440081, -13.76003991320737541, -219.7405193562604495 ) ) ;
#4430 = ITEM_DEFINED_TRANSFORMATION ( 'NONE', 'NONE', #1257,  #6677 ) ;
#4431 = CARTESIAN_POINT ( 'NONE',  ( -3.003186468682855104, 15.63968344752823469, -231.5301608670590667 ) ) ;
#4432 = CARTESIAN_POINT ( 'NONE',  ( 0.1645309800062008665, 15.56029994314186382, -233.1129172884685943 ) ) ;
#4433 = EDGE_LOOP ( 'NONE', ( #1402, #5404, #7386, #10652 ) ) ;
#4434 = CARTESIAN_POINT ( 'NONE',  ( -17.75316132689678383, 25.03468689048078843, -222.1645193425721061 ) ) ;
#4435 = CARTESIAN_POINT ( 'NONE',  ( -19.29805292978571885, -8.785194383212417080, -233.3520286081516133 ) ) ;
#4436 = CARTESIAN_POINT ( 'NONE',  ( -24.74809011923674262, -3.553243708740094320, -9.353164043501660530 ) ) ;
#4437 = DIRECTION ( 'NONE',  ( 1.000000000000000000, 0.000000000000000000, 0.000000000000000000 ) ) ;
#4438 = CARTESIAN_POINT ( 'NONE',  ( -10.24288955603410933, 28.30762631303078791, -220.8855665231519083 ) ) ;
#4439 = CARTESIAN_POINT ( 'NONE',  ( -6.646164377397596468, -30.92684034042379437, -222.9942643485979374 ) ) ;
#4440 = CARTESIAN_POINT ( 'NONE',  ( 15.84759643368428428, -7.142586963752317608, -231.1761396821659673 ) ) ;
#4441 = CARTESIAN_POINT ( 'NONE',  ( -14.83974801774860630, 13.71714848582103485, -216.0935642439352762 ) ) ;
#4442 = CARTESIAN_POINT ( 'NONE',  ( -30.35034897870229287, 7.696526532841741819, -221.5749790623549416 ) ) ;
#4443 = EDGE_CURVE ( 'NONE', #17126, #4726, #6051, .T. ) ;
#4444 = CARTESIAN_POINT ( 'NONE',  ( -1.386728072030569692, 16.52832439466973824, -230.7516952943509807 ) ) ;
#4445 = DIRECTION ( 'NONE',  ( 0.000000000000000000, -1.000000000000000000, 0.000000000000000000 ) ) ;
#4446 = CARTESIAN_POINT ( 'NONE',  ( -17.17981675979428147, 1.478343374046288128, -216.2419730925687418 ) ) ;
#4447 = CARTESIAN_POINT ( 'NONE',  ( -7.069738587058329138, -16.45101055981254845, -220.5392980307454138 ) ) ;
#4448 = ORIENTED_EDGE ( 'NONE', *, *, #14092, .F. ) ;
#4449 = CARTESIAN_POINT ( 'NONE',  ( -11.05032764129755840, 11.65053160594169945, -221.1796278216217218 ) ) ;
#4450 = CARTESIAN_POINT ( 'NONE',  ( 7.450672702945051462, 17.42371045663376705, -217.2894981592719432 ) ) ;
#4451 = CARTESIAN_POINT ( 'NONE',  ( -5.566280468132954518, 29.91920859341914962, -222.2705790733167817 ) ) ;
#4452 = ORIENTED_EDGE ( 'NONE', *, *, #1949, .F. ) ;
#4453 = CARTESIAN_POINT ( 'NONE',  ( 26.38334502096500245, -3.352420239867627494, -217.3603908026431384 ) ) ;
#4454 = ADVANCED_FACE ( 'NONE', ( #14366 ), #4972, .T. ) ;
#4455 = DIRECTION ( 'NONE',  ( -1.000000000000000000, 0.000000000000000000, 0.000000000000000000 ) ) ;
#4456 = ORIENTED_EDGE ( 'NONE', *, *, #17479, .T. ) ;
#4457 = CARTESIAN_POINT ( 'NONE',  ( -27.82842955277035202, 11.70195273568964112, -227.9294339757464911 ) ) ;
#4458 = CARTESIAN_POINT ( 'NONE',  ( -20.34211109426514597, -24.21145056749966074, -225.0780941718357724 ) ) ;
#4459 = CARTESIAN_POINT ( 'NONE',  ( 28.51464931495100785, 5.422321182929326966, -223.8116416110474347 ) ) ;
#4460 = AXIS2_PLACEMENT_3D ( 'NONE', #1551, #11797, #3224 ) ;
#4461 = CARTESIAN_POINT ( 'NONE',  ( 22.84140515590350518, 18.29101041979067332, -226.2334522600520472 ) ) ;
#4462 = CARTESIAN_POINT ( 'NONE',  ( 14.67485956688574689, -3.005730394301288744, -224.9297226343007594 ) ) ;
#4463 = UNCERTAINTY_MEASURE_WITH_UNIT (LENGTH_MEASURE( 1.000000000000000082E-05 ), #10987, 'distance_accuracy_value', 'NONE');
#4464 = CARTESIAN_POINT ( 'NONE',  ( -19.50431861204945605, -0.7624880359591150736, -219.4666829195064395 ) ) ;
#4465 = CARTESIAN_POINT ( 'NONE',  ( 17.04685026979186446, 18.05617612716381970, -216.0910122987878310 ) ) ;
#4466 = FILL_AREA_STYLE_COLOUR ( '', #11691 ) ;
#4467 = CARTESIAN_POINT ( 'NONE',  ( -24.60613290926164609, 4.462958844126968749, -8.973150446544476466 ) ) ;
#4468 = CARTESIAN_POINT ( 'NONE',  ( 17.00168025137501004, 6.212099629982537508, -219.0548246536471595 ) ) ;
#4469 = CARTESIAN_POINT ( 'NONE',  ( 0.000000000000000000, 0.000000000000000000, -105.0000000000000142 ) ) ;
#4470 = CARTESIAN_POINT ( 'NONE',  ( 21.58416078958130413, -8.344710983103166058, -219.2549068428508861 ) ) ;
#4471 = EDGE_CURVE ( 'NONE', #7333, #3862, #7868, .T. ) ;
#4472 = CARTESIAN_POINT ( 'NONE',  ( -18.53787071664277519, -6.556543064843903146, -232.5192140591401824 ) ) ;
#4473 = DIRECTION ( 'NONE',  ( 0.000000000000000000, 0.000000000000000000, -1.000000000000000000 ) ) ;
#4474 = CIRCLE ( 'NONE', #522, 3.000000000000002665 ) ;
#4475 = CARTESIAN_POINT ( 'NONE',  ( 0.000000000000000000, 21.00000000000000000, -75.00000000000000000 ) ) ;
#4476 = CARTESIAN_POINT ( 'NONE',  ( -1.973645837583506424, 28.78841935349527503, -228.5341874691134763 ) ) ;
#4477 = CARTESIAN_POINT ( 'NONE',  ( 15.86371404000427887, -2.776058937659206638, -233.1947532464443213 ) ) ;
#4478 = CARTESIAN_POINT ( 'NONE',  ( 14.62702828724412285, -1.994068170757606673, -224.0552340365271959 ) ) ;
#4479 = MECHANICAL_DESIGN_GEOMETRIC_PRESENTATION_REPRESENTATION (  '', ( #21017 ), #12765 ) ;
#4480 = CARTESIAN_POINT ( 'NONE',  ( -20.45797657813638182, 1.164962349958370336, -217.1306074022350572 ) ) ;
#4481 = CARTESIAN_POINT ( 'NONE',  ( 28.65393683769942967, 4.398063292302325067, -219.1542358361629965 ) ) ;
#4482 = CARTESIAN_POINT ( 'NONE',  ( 10.79895562092076844, 12.01490073542734116, -225.7380208924852809 ) ) ;
#4483 = VERTEX_POINT ( 'NONE', #18176 ) ;
#4484 = CARTESIAN_POINT ( 'NONE',  ( 3.099569060413221333, -25.61866983817578713, -217.9657659276338677 ) ) ;
#4485 = CARTESIAN_POINT ( 'NONE',  ( 0.06328415631827062626, 14.50030254718124212, 92.99999999999997158 ) ) ;
#4486 = CARTESIAN_POINT ( 'NONE',  ( -12.36382104905844592, -0.1264132474004772688, -228.0034406263598896 ) ) ;
#4487 = CARTESIAN_POINT ( 'NONE',  ( -4.154119475380428916, 11.54776298361823095, -227.0876712548254943 ) ) ;
#4488 = CARTESIAN_POINT ( 'NONE',  ( 7.587775680576782200, 20.81864918083767435, -235.2547171215352364 ) ) ;
#4489 = CARTESIAN_POINT ( 'NONE',  ( 13.37416304104233333, -8.359606308866407431, -226.7674924273047452 ) ) ;
#4490 = CARTESIAN_POINT ( 'NONE',  ( -0.3969026096611234511, 20.89748314411456676, -216.3289738411752978 ) ) ;
#4491 = CARTESIAN_POINT ( 'NONE',  ( 0.000000000000000000, 0.000000000000000000, -55.00000000000000000 ) ) ;
#4492 = VECTOR ( 'NONE', #6161, 1000.000000000000000 ) ;
#4493 = CARTESIAN_POINT ( 'NONE',  ( -6.260151855817680300, 29.88549235135308635, -226.8929519981915064 ) ) ;
#4494 = CIRCLE ( 'NONE', #13494, 3.000000000000002665 ) ;
#4495 = CARTESIAN_POINT ( 'NONE',  ( -28.05279008194460744, 4.018900919424986284, -224.6698354068587662 ) ) ;
#4496 = CARTESIAN_POINT ( 'NONE',  ( -16.39453490553961856, 20.24836633112041184, -233.1722131570092245 ) ) ;
#4497 = CARTESIAN_POINT ( 'NONE',  ( 13.43730899468209294, 8.427513769504761498, -221.4030804848920297 ) ) ;
#4498 = CARTESIAN_POINT ( 'NONE',  ( 3.182992543297812560, 16.68308636702302650, -221.9272281984358415 ) ) ;
#4499 = CARTESIAN_POINT ( 'NONE',  ( 0.000000000000000000, 0.000000000000000000, -70.00000000000000000 ) ) ;
#4500 = CARTESIAN_POINT ( 'NONE',  ( 8.858651440950676914, 22.47383302477780376, -230.7859943773311215 ) ) ;
#4501 = CARTESIAN_POINT ( 'NONE',  ( -14.13781561609191328, -15.90667165809925621, -233.6615929499251649 ) ) ;
#4502 = CARTESIAN_POINT ( 'NONE',  ( 18.04365516558436866, 6.721233635139160612, -218.4376093631473168 ) ) ;
#4503 = CARTESIAN_POINT ( 'NONE',  ( -3.300732473188277005, -24.68991359470437175, -216.3853901891898488 ) ) ;
#4504 = CARTESIAN_POINT ( 'NONE',  ( -7.464187997994982560, 14.20693289415472016, -228.8865298551900764 ) ) ;
#4505 = CARTESIAN_POINT ( 'NONE',  ( 25.09678678204237201, -16.96620885351193309, -225.7902784465786965 ) ) ;
#4506 = CARTESIAN_POINT ( 'NONE',  ( 18.13412043358480474, 12.55378873098427128, -233.2186159706515696 ) ) ;
#4507 = CARTESIAN_POINT ( 'NONE',  ( -8.435479365662203577, 14.12888021429238528, -220.5365774424437859 ) ) ;
#4508 = CARTESIAN_POINT ( 'NONE',  ( -18.07648963816576781, 14.36622924931724654, -235.1425738388569187 ) ) ;
#4509 = CARTESIAN_POINT ( 'NONE',  ( -21.34127571194312623, -5.850660018714998856, -219.1209233896074977 ) ) ;
#4510 = AXIS2_PLACEMENT_3D ( 'NONE', #16453, #4178, #914 ) ;
#4511 = CARTESIAN_POINT ( 'NONE',  ( -16.66921372850992000, 0.4301828684420727078, -227.8397539831347842 ) ) ;
#4512 = CARTESIAN_POINT ( 'NONE',  ( 2.000000000000000000, 0.000000000000000000, -120.0000000000000142 ) ) ;
#4513 = CARTESIAN_POINT ( 'NONE',  ( -24.74482344071061135, -7.641957171360318490, -233.9284114646162891 ) ) ;
#4514 = CARTESIAN_POINT ( 'NONE',  ( 2.808299412262623473, 18.06245856371233316, -217.9832661743849656 ) ) ;
#4515 = CARTESIAN_POINT ( 'NONE',  ( 29.55842656951424985, 4.785221541509360854, -220.5134865854112718 ) ) ;
#4516 = CARTESIAN_POINT ( 'NONE',  ( -9.007976471255481954, 12.60968992764439633, -227.9367755778692981 ) ) ;
#4517 = CARTESIAN_POINT ( 'NONE',  ( 3.982203626615636427, 14.63895582687697150, -217.4952312584269123 ) ) ;
#4518 = COLOUR_RGB ( '', 0.66274510, 0.83137255, 0.94901961) ;
#4519 = ORIENTED_EDGE ( 'NONE', *, *, #14391, .T. ) ;
#4520 = CARTESIAN_POINT ( 'NONE',  ( -3.664580975482237157, -26.87662451849047329, -230.7630177344243236 ) ) ;
#4521 = ADVANCED_FACE ( 'NONE', ( #4210, #21637 ), #16260, .F. ) ;
#4522 = EDGE_LOOP ( 'NONE', ( #7478, #7056, #20532, #1416, #18568 ) ) ;
#4523 = CARTESIAN_POINT ( 'NONE',  ( 0.9095753368782393267, -25.50589708844611891, -231.1945442011520697 ) ) ;
#4524 = CARTESIAN_POINT ( 'NONE',  ( -27.68973657932738064, 5.930811633061950694, -216.7842770206311513 ) ) ;
#4525 = CARTESIAN_POINT ( 'NONE',  ( 13.49882595795384255, -9.201056071450322449, -219.2439763087855908 ) ) ;
#4526 = CARTESIAN_POINT ( 'NONE',  ( -26.43144772945995413, -6.745116643720071359, -219.5134289301136050 ) ) ;
#4527 = CARTESIAN_POINT ( 'NONE',  ( -11.39823187951283501, -7.998194509987097689, -226.8062974464413912 ) ) ;
#4528 = APPLICATION_CONTEXT ( 'automotive_design' ) ;
#4529 = CARTESIAN_POINT ( 'NONE',  ( 9.214796078729456497, 26.59493510027307650, -225.5796848805584318 ) ) ;
#4530 = DIRECTION ( 'NONE',  ( 0.000000000000000000, 0.000000000000000000, -1.000000000000000000 ) ) ;
#4531 = DIRECTION ( 'NONE',  ( 0.000000000000000000, 0.000000000000000000, -1.000000000000000000 ) ) ;
#4532 = CARTESIAN_POINT ( 'NONE',  ( -13.44241955326339166, 15.88952131657459965, -217.2587743382015901 ) ) ;
#4533 = CARTESIAN_POINT ( 'NONE',  ( 5.248230734842167955, 23.54336384919183445, -216.8914391693808739 ) ) ;
#4534 = CARTESIAN_POINT ( 'NONE',  ( 8.632180352507942800, 16.83956698119041917, -230.4752415867875186 ) ) ;
#4535 = CARTESIAN_POINT ( 'NONE',  ( 17.05764047735875266, -11.29112887239367424, -214.9748062598841898 ) ) ;
#4536 = CARTESIAN_POINT ( 'NONE',  ( 16.96779410054824666, 23.69881408353223406, -220.2174342377987841 ) ) ;
#4537 = CARTESIAN_POINT ( 'NONE',  ( -17.00819119081011266, 8.904695857470725784, -219.7915043529501133 ) ) ;
#4538 = CARTESIAN_POINT ( 'NONE',  ( -25.48569860171343748, 4.299098795181173216, -219.7804659532078801 ) ) ;
#4539 = CARTESIAN_POINT ( 'NONE',  ( 3.619268272960482591, -21.10655420957111517, -217.8630709410095108 ) ) ;
#4540 = DIRECTION ( 'NONE',  ( 0.000000000000000000, 0.000000000000000000, -1.000000000000000000 ) ) ;
#4541 = CARTESIAN_POINT ( 'NONE',  ( 24.99999999999999645, 3.061616997868383437E-15, -224.9999999999999716 ) ) ;
#4542 = CARTESIAN_POINT ( 'NONE',  ( 14.32085100525799248, 9.220655089380342062, -219.9006227404039464 ) ) ;
#4543 = CARTESIAN_POINT ( 'NONE',  ( 15.00179858758994911, -7.185045179863253750, -227.1671253934038077 ) ) ;
#4544 = FACE_BOUND ( 'NONE', #13844, .T. ) ;
#4545 = CARTESIAN_POINT ( 'NONE',  ( -8.803769170443210612, -17.82266517633203406, -233.6972128408098683 ) ) ;
#4546 = PRODUCT_CONTEXT ( 'NONE', #7149, 'mechanical' ) ;
#4547 = CARTESIAN_POINT ( 'NONE',  ( -4.620781219515533778, 16.99182040716223696, -217.1278208835672672 ) ) ;
#4548 = CARTESIAN_POINT ( 'NONE',  ( 3.641537757978871248, 12.43698445400491437, -220.3805014257186485 ) ) ;
#4549 = ORIENTED_EDGE ( 'NONE', *, *, #6961, .T. ) ;
#4550 = CARTESIAN_POINT ( 'NONE',  ( -3.514547081416551588, 30.38636916157537016, -227.3529586180979436 ) ) ;
#4551 = CARTESIAN_POINT ( 'NONE',  ( -22.25980993584449408, -3.522148912989541802, -233.7954546715351398 ) ) ;
#4552 = CARTESIAN_POINT ( 'NONE',  ( 1.232595164407830946E-29, -17.50000000000007105, -60.00000000000000000 ) ) ;
#4553 = CARTESIAN_POINT ( 'NONE',  ( 4.100000000000000533, 0.000000000000000000, -126.0000000000000284 ) ) ;
#4554 = CARTESIAN_POINT ( 'NONE',  ( 3.763426558366607111, 28.60172112197566818, -230.1816715025297526 ) ) ;
#4555 = CARTESIAN_POINT ( 'NONE',  ( -4.110806133445755961, -12.94090688063470473, -230.1197724001632992 ) ) ;
#4556 = CARTESIAN_POINT ( 'NONE',  ( 15.33694643395292090, -2.540932720676567502, -228.3777194553126435 ) ) ;
#4557 = CARTESIAN_POINT ( 'NONE',  ( -9.716674560061926869, 27.56227806819028103, -219.4917914922789919 ) ) ;
#4558 = CARTESIAN_POINT ( 'NONE',  ( 14.32363442937021425, 2.978337679677412808, -227.0386046113487453 ) ) ;
#4559 = CARTESIAN_POINT ( 'NONE',  ( -4.211886032913159106, 20.62037006687756602, -216.9488349035050305 ) ) ;
#4560 = CARTESIAN_POINT ( 'NONE',  ( -16.71711190488355570, 0.6105529133557690002, -230.9511258789794681 ) ) ;
#4561 = CARTESIAN_POINT ( 'NONE',  ( 27.30736127486511577, 7.960716467858479639, -228.6121938484450595 ) ) ;
#4562 = CARTESIAN_POINT ( 'NONE',  ( -13.78780214743967214, -7.867619234746639378, -226.3818292120506044 ) ) ;
#4563 = ADVANCED_FACE ( 'NONE', ( #622 ), #9295, .F. ) ;
#4564 = VERTEX_POINT ( 'NONE', #16051 ) ;
#4565 = CARTESIAN_POINT ( 'NONE',  ( -10.30870167223346456, 11.95603877111467561, -228.4123369090513336 ) ) ;
#4566 = CARTESIAN_POINT ( 'NONE',  ( 5.359747511823000465, 20.14556701535824601, -232.9094821222151381 ) ) ;
#4567 = CARTESIAN_POINT ( 'NONE',  ( -6.127117917506272882, 18.94558806480136681, -232.9763641438055117 ) ) ;
#4568 = CARTESIAN_POINT ( 'NONE',  ( 13.37423534347618670, -3.100899090186935325, -222.2483675785374260 ) ) ;
#4569 = CARTESIAN_POINT ( 'NONE',  ( 0.000000000000000000, 0.000000000000000000, 75.00000000000000000 ) ) ;
#4570 = ORIENTED_EDGE ( 'NONE', *, *, #14092, .T. ) ;
#4571 = CARTESIAN_POINT ( 'NONE',  ( -11.24282496690421596, 12.44430180464951086, -232.4405891940542404 ) ) ;
#4572 = CARTESIAN_POINT ( 'NONE',  ( -4.241635020808209866, -19.61639137582426429, -216.9458228475819226 ) ) ;
#4573 = CARTESIAN_POINT ( 'NONE',  ( 17.07668571305246985, 2.037405138410691485, -219.7626854147787867 ) ) ;
#4574 = CARTESIAN_POINT ( 'NONE',  ( 10.50530447320976535, 20.19629329636330084, -217.1354359361034767 ) ) ;
#4575 = CARTESIAN_POINT ( 'NONE',  ( 25.00000000000001066, -3.061616997868384226E-15, -75.00000000000000000 ) ) ;
#4576 = ADVANCED_FACE ( 'NONE', ( #7498 ), #14585, .T. ) ;
#4577 = CARTESIAN_POINT ( 'NONE',  ( -19.18087294808806931, 21.32275554655070593, -230.8558978902391061 ) ) ;
#4578 = CARTESIAN_POINT ( 'NONE',  ( 17.66865342763861690, 2.849170916951684784, -230.9175656266857004 ) ) ;
#4579 = CARTESIAN_POINT ( 'NONE',  ( 0.000000000000000000, 0.000000000000000000, 89.13175911166534604 ) ) ;
#4580 = CARTESIAN_POINT ( 'NONE',  ( 20.58703255433590940, 0.4816031003617209372, -231.9427175861361263 ) ) ;
#4581 = CARTESIAN_POINT ( 'NONE',  ( 1.322875655532295358, 1.500000000000000000, -378.2244600276337678 ) ) ;
#4582 = CARTESIAN_POINT ( 'NONE',  ( 28.03541074264261113, -3.118360251426135488, -224.4433144283077581 ) ) ;
#4583 = CARTESIAN_POINT ( 'NONE',  ( -13.33530847390368024, -5.065163879519744228, -226.5386329521395226 ) ) ;
#4584 = DIRECTION ( 'NONE',  ( -0.000000000000000000, 0.000000000000000000, -1.000000000000000000 ) ) ;
#4585 = DIRECTION ( 'NONE',  ( -1.000000000000000000, 0.000000000000000000, 0.000000000000000000 ) ) ;
#4586 = CARTESIAN_POINT ( 'NONE',  ( -15.64710113362562183, 25.90300453978063189, -220.8637308366217269 ) ) ;
#4587 = CARTESIAN_POINT ( 'NONE',  ( 28.26377063890550190, -1.722554810693586180, -217.1290174754948623 ) ) ;
#4588 = CARTESIAN_POINT ( 'NONE',  ( 19.63495056682994289, -4.096126682090319271, -232.1271738766904207 ) ) ;
#4589 = CARTESIAN_POINT ( 'NONE',  ( -20.00523085820573499, 3.356386534894876927, -232.9491364426554298 ) ) ;
#4590 = CARTESIAN_POINT ( 'NONE',  ( -16.04492519386327487, 1.819644280589142626, -223.4665098021627614 ) ) ;
#4591 = CARTESIAN_POINT ( 'NONE',  ( 16.48099188159542194, 16.04875567542346815, -230.8408106201084706 ) ) ;
#4592 = ORIENTED_EDGE ( 'NONE', *, *, #6914, .F. ) ;
#4593 = CARTESIAN_POINT ( 'NONE',  ( 12.79824285610881063, -25.13061632922516253, -232.1172912921500426 ) ) ;
#4594 = CARTESIAN_POINT ( 'NONE',  ( -13.27786176931083162, 6.453512288987280243, 92.99999999999998579 ) ) ;
#4595 = CARTESIAN_POINT ( 'NONE',  ( -26.42613204384124259, 13.88327151024443395, -218.2510073314678323 ) ) ;
#4596 = CARTESIAN_POINT ( 'NONE',  ( 7.587775680576782200, 20.81864918083767435, -235.2547171215352364 ) ) ;
#4597 = CARTESIAN_POINT ( 'NONE',  ( 3.714886539878811789, 12.88803176524806560, -219.5889136906770034 ) ) ;
#4598 = CARTESIAN_POINT ( 'NONE',  ( 15.59528062753244804, -5.679035096727840681, -230.0190217829878918 ) ) ;
#4599 = CARTESIAN_POINT ( 'NONE',  ( -17.17400284685640344, 24.63223427531467280, -220.6313524368512162 ) ) ;
#4600 = CARTESIAN_POINT ( 'NONE',  ( -18.71530386740073126, -0.6857509888707814527, -217.6195632122020527 ) ) ;
#4601 = EDGE_CURVE ( 'NONE', #11033, #21666, #20906, .T. ) ;
#4602 = VECTOR ( 'NONE', #9071, 1000.000000000000000 ) ;
#4603 = CARTESIAN_POINT ( 'NONE',  ( 5.264801124131998300, 10.54092478143144795, -226.4890466082630098 ) ) ;
#4604 = CARTESIAN_POINT ( 'NONE',  ( -18.94444594796027914, 3.458349568010113728, -218.9807021659310635 ) ) ;
#4605 = CARTESIAN_POINT ( 'NONE',  ( -14.70651859537745487, 4.211702956367679107, -230.0357207626005334 ) ) ;
#4606 = CARTESIAN_POINT ( 'NONE',  ( 28.57344184061583192, 5.631897254180425527, -225.1192013637692355 ) ) ;
#4607 = CARTESIAN_POINT ( 'NONE',  ( 3.786538429322381383, 16.06208591393598084, -226.9891439814428793 ) ) ;
#4608 = FACE_OUTER_BOUND ( 'NONE', #9012, .T. ) ;
#4609 = DIRECTION ( 'NONE',  ( 0.000000000000000000, -0.7999999999999997113, 0.6000000000000004219 ) ) ;
#4610 = CARTESIAN_POINT ( 'NONE',  ( 10.73846460100926592, 12.62787417135106161, -222.6344468496098159 ) ) ;
#4611 = CARTESIAN_POINT ( 'NONE',  ( -12.44777057840899559, -8.577008958641105352, -229.4809580173677830 ) ) ;
#4612 = CARTESIAN_POINT ( 'NONE',  ( 14.54149994592679107, 8.070685273005897997, -229.7292930672863349 ) ) ;
#4613 = CARTESIAN_POINT ( 'NONE',  ( 4.525470981882147470, -27.64997114140619416, -217.1529231092339103 ) ) ;
#4614 = CARTESIAN_POINT ( 'NONE',  ( 25.50000000000000000, 0.000000000000000000, 0.000000000000000000 ) ) ;
#4615 = CARTESIAN_POINT ( 'NONE',  ( -14.22255565734842619, 21.32307452572284134, -218.8849463683180261 ) ) ;
#4616 = DIRECTION ( 'NONE',  ( -0.000000000000000000, 0.000000000000000000, -1.000000000000000000 ) ) ;
#4617 = CARTESIAN_POINT ( 'NONE',  ( 16.26147397530412420, -13.20473954510486081, -216.9283256773164794 ) ) ;
#4618 = CARTESIAN_POINT ( 'NONE',  ( 9.125049424194871861, 12.37796447639467523, -227.2539065556229332 ) ) ;
#4619 = CARTESIAN_POINT ( 'NONE',  ( -14.87932799058895128, 18.71706570923887369, -231.8731726670167745 ) ) ;
#4621 = TOROIDAL_SURFACE ( 'NONE', #6424, 22.00000000000000711, 2.999999999999999112 ) ;
#4620 = CARTESIAN_POINT ( 'NONE',  ( -22.61701582078733708, 5.416317966792455252, -214.6955127214549748 ) ) ;
#4622 = CARTESIAN_POINT ( 'NONE',  ( -15.27576489228250090, -6.235258113955679526, -227.2120396213316553 ) ) ;
#4623 = CARTESIAN_POINT ( 'NONE',  ( -19.50431861204945605, -0.7624880359591150736, -219.4666829195064395 ) ) ;
#4624 = CARTESIAN_POINT ( 'NONE',  ( 0.000000000000000000, 0.000000000000000000, 75.00000000000000000 ) ) ;
#4625 = CARTESIAN_POINT ( 'NONE',  ( -14.44949936980387584, -0.9990553581641278269, -220.3450678990494964 ) ) ;
#4626 = CARTESIAN_POINT ( 'NONE',  ( 14.20064147608437821, 14.63411858269657806, -233.6150408276221242 ) ) ;
#4627 = CARTESIAN_POINT ( 'NONE',  ( 25.38325563848796662, 11.05100313887457553, -217.8685524735130628 ) ) ;
#4628 = CARTESIAN_POINT ( 'NONE',  ( -1.884624261322229266, 13.00421381464247084, -226.7648460381863345 ) ) ;
#4629 = CARTESIAN_POINT ( 'NONE',  ( 4.849508625227819003, 24.02665844953846275, -214.9607406399067315 ) ) ;
#4630 = B_SPLINE_CURVE_WITH_KNOTS ( 'NONE', 3,
 ( #5807, #16284, #21114, #533, #4230, #9420 ),
 .UNSPECIFIED., .F., .F.,
 ( 4, 2, 4 ),
 ( 0.003413498328254622755, 0.003630484103855696840, 0.003847469879456770925 ),
 .UNSPECIFIED. ) ;
#4631 = CARTESIAN_POINT ( 'NONE',  ( 6.833096512853454207, -24.74801519961247465, -219.7405977492105364 ) ) ;
#4632 = ORIENTED_EDGE ( 'NONE', *, *, #7205, .F. ) ;
#4633 = CARTESIAN_POINT ( 'NONE',  ( 1.268102448827562068, -18.18084990330622830, -231.0699201170278911 ) ) ;
#4634 = CARTESIAN_POINT ( 'NONE',  ( -9.924247690135956645, 7.079756654796299564, -222.1205998075789694 ) ) ;
#4635 = CARTESIAN_POINT ( 'NONE',  ( 25.46470895113276711, -14.41152162994631070, -228.1811935238409035 ) ) ;
#4636 = CARTESIAN_POINT ( 'NONE',  ( 27.83450977899788370, 1.364662819714677511, -230.5442677252456463 ) ) ;
#4637 = CARTESIAN_POINT ( 'NONE',  ( -20.11874861854083463, -21.11755179634840474, -229.7504124090357323 ) ) ;
#4638 = CARTESIAN_POINT ( 'NONE',  ( 14.19979467405507556, 6.351366891014061267, -230.8614099669030679 ) ) ;
#4639 = EDGE_CURVE ( 'NONE', #8365, #16840, #5448, .T. ) ;
#4640 = CARTESIAN_POINT ( 'NONE',  ( -15.72555926117677139, 17.60926865496976745, -217.2114552733360142 ) ) ;
#4641 = CARTESIAN_POINT ( 'NONE',  ( 20.54489901492447501, 10.52141067440427591, -216.2005526543161693 ) ) ;
#4642 = CARTESIAN_POINT ( 'NONE',  ( 5.343558017910363667, 26.29639771561252459, -218.1010331760174665 ) ) ;
#4643 = CARTESIAN_POINT ( 'NONE',  ( 13.88312867625433711, 12.44451767566605760, -217.7066242262208391 ) ) ;
#4644 = CARTESIAN_POINT ( 'NONE',  ( 6.910796951316678260, -9.495606915386650471, -226.6778026831113380 ) ) ;
#4645 = CARTESIAN_POINT ( 'NONE',  ( 15.91624278015930649, 5.932232821383347954, -217.3600859879243217 ) ) ;
#4646 = CARTESIAN_POINT ( 'NONE',  ( -6.581016643627174645, 27.50493254600863935, -230.8763182197739070 ) ) ;
#4647 = CARTESIAN_POINT ( 'NONE',  ( -12.58820391453271093, -22.27128923838312247, -218.3899974299303324 ) ) ;
#4648 = DIRECTION ( 'NONE',  ( 0.000000000000000000, 0.000000000000000000, -1.000000000000000000 ) ) ;
#4649 = DIRECTION ( 'NONE',  ( 0.000000000000000000, 0.000000000000000000, -1.000000000000000000 ) ) ;
#4650 = CARTESIAN_POINT ( 'NONE',  ( 18.04365516558436866, 6.721233635139160612, -218.4376093631473168 ) ) ;
#4651 = CARTESIAN_POINT ( 'NONE',  ( 23.68557655437113141, -13.81416892717991551, -227.4080549258873987 ) ) ;
#4652 = EDGE_CURVE ( 'NONE', #10566, #20364, #2228, .T. ) ;
#4653 = CARTESIAN_POINT ( 'NONE',  ( -13.88743542672353826, 10.36310385030668613, -230.6144170796622745 ) ) ;
#4654 = CARTESIAN_POINT ( 'NONE',  ( -4.670971249126254499, -22.80666086768999890, -234.0323572959307512 ) ) ;
#4655 = CARTESIAN_POINT ( 'NONE',  ( 13.19406830060760605, 4.163358546877222288, -228.8532745215267425 ) ) ;
#4656 = CARTESIAN_POINT ( 'NONE',  ( 4.966801760238292118, 27.41406605988239420, -216.4490579899774900 ) ) ;
#4657 = ORIENTED_EDGE ( 'NONE', *, *, #13403, .T. ) ;
#4658 = CARTESIAN_POINT ( 'NONE',  ( -2.958555384449997661, 13.07587799061801093, -222.7767538261418565 ) ) ;
#4659 = CARTESIAN_POINT ( 'NONE',  ( -17.04082806826102470, -4.797954729550726327, -217.3726213297937306 ) ) ;
#4660 = CARTESIAN_POINT ( 'NONE',  ( -23.84329938582383690, -7.531468209848477535, -6.610083113334743743 ) ) ;
#4661 = DIRECTION ( 'NONE',  ( -0.000000000000000000, -0.000000000000000000, 1.000000000000000000 ) ) ;
#4662 = CARTESIAN_POINT ( 'NONE',  ( -2.772442535524381579, 13.75675912271027457, -228.9770533867650215 ) ) ;
#4663 = CARTESIAN_POINT ( 'NONE',  ( -7.876537541093066253, -10.96045937405908965, -230.9151686379251487 ) ) ;
#4664 = CARTESIAN_POINT ( 'NONE',  ( 12.02378739738799140, -16.98783239109716092, -233.4545636224233931 ) ) ;
#4665 = CARTESIAN_POINT ( 'NONE',  ( 28.36095019830170472, -8.296631283839911220, -225.2861439608085448 ) ) ;
#4666 = CARTESIAN_POINT ( 'NONE',  ( -19.94037810645588138, 20.40093185429846656, -220.0593903119159620 ) ) ;
#4667 = CARTESIAN_POINT ( 'NONE',  ( 11.00580183749007190, 25.74996642444834904, -225.8602305833924788 ) ) ;
#4668 = CARTESIAN_POINT ( 'NONE',  ( -29.88125065636863198, 4.504452993877526623, -226.2048141718237275 ) ) ;
#4669 = CARTESIAN_POINT ( 'NONE',  ( -15.00242079508237936, 7.335218745534954898, -232.9526071471669013 ) ) ;
#4670 = CARTESIAN_POINT ( 'NONE',  ( -13.11077419447928349, -11.05578789306379406, -228.2719546787038212 ) ) ;
#4671 = CARTESIAN_POINT ( 'NONE',  ( -4.583529401292260275, 28.77615850237956607, -226.7744741901706504 ) ) ;
#4672 = CARTESIAN_POINT ( 'NONE',  ( 13.10956039622986324, 4.581323766968698585, -221.0328522389722252 ) ) ;
#4673 = CARTESIAN_POINT ( 'NONE',  ( 2.471991688031208945, 13.88348721647344419, -230.6707754746932437 ) ) ;
#4674 = CARTESIAN_POINT ( 'NONE',  ( 24.64273247744971229, -10.07127014888436278, -217.7281412196979602 ) ) ;
#4675 = DIRECTION ( 'NONE',  ( 0.000000000000000000, 0.000000000000000000, 1.000000000000000000 ) ) ;
#4676 = ORIENTED_EDGE ( 'NONE', *, *, #983, .T. ) ;
#4677 = CARTESIAN_POINT ( 'NONE',  ( -23.49379658590067876, 11.46840048879614393, -217.2519070826072323 ) ) ;
#4678 = CARTESIAN_POINT ( 'NONE',  ( -11.17605908769978740, -26.51801958233905765, -230.6004191093659301 ) ) ;
#4679 = CARTESIAN_POINT ( 'NONE',  ( 14.63113973005795643, 4.926264598692385199, -222.4866305912601945 ) ) ;
#4680 = CARTESIAN_POINT ( 'NONE',  ( 4.656903975822286768, 13.45000048768594780, -227.6722060245555497 ) ) ;
#4681 = DIRECTION ( 'NONE',  ( -2.162300680179923768E-16, -1.000000000000000000, 0.000000000000000000 ) ) ;
#4682 = PRODUCT_DEFINITION_CONTEXT ( 'detailed design', #12889, 'design' ) ;
#4683 = CARTESIAN_POINT ( 'NONE',  ( -2.465190328815661892E-29, -25.00000000000012790, 75.00000000000000000 ) ) ;
#4684 = CARTESIAN_POINT ( 'NONE',  ( -17.20794623181132721, 21.97849129791581291, -217.9187454682870850 ) ) ;
#4685 = EDGE_CURVE ( 'NONE', #324, #12893, #18393, .T. ) ;
#4686 = CARTESIAN_POINT ( 'NONE',  ( 16.10828274231666768, 3.530956590605524692, -220.6574330336208050 ) ) ;
#4687 = CARTESIAN_POINT ( 'NONE',  ( -23.33796567949162082, 8.964750604579641902, -4.443019783309294368 ) ) ;
#4688 = CARTESIAN_POINT ( 'NONE',  ( 21.82670294635402897, -0.1727854921979527503, -222.0037445873432205 ) ) ;
#4689 = CARTESIAN_POINT ( 'NONE',  ( -21.08008464085897060, -0.9048411197481797119, -217.0000000010748522 ) ) ;
#4690 = CARTESIAN_POINT ( 'NONE',  ( 26.31881739696682843, -8.664992621510689830, -226.4435203923285655 ) ) ;
#4691 = CARTESIAN_POINT ( 'NONE',  ( -16.20471097821853235, -2.781505378741172319, -220.1484675126197317 ) ) ;
#4692 = CYLINDRICAL_SURFACE ( 'NONE', #20597, 21.00000000000008171 ) ;
#4693 = LINE ( 'NONE', #175, #9110 ) ;
#4694 = CARTESIAN_POINT ( 'NONE',  ( 1.847452069095833593, 15.11597492720254543, -223.6261404253179421 ) ) ;
#4695 = CARTESIAN_POINT ( 'NONE',  ( 12.44757525125794118, -27.84495572490402182, -221.5053358145852656 ) ) ;
#4696 = CARTESIAN_POINT ( 'NONE',  ( 15.60497028854143764, -26.39208911975253002, -225.8550158017044112 ) ) ;
#4697 = CARTESIAN_POINT ( 'NONE',  ( -18.88895772509644644, 1.306698388790553444, -217.6272550812279292 ) ) ;
#4698 = CARTESIAN_POINT ( 'NONE',  ( 21.96352831578506937, -0.3315607655626218175, -233.9427286327412787 ) ) ;
#4699 = CARTESIAN_POINT ( 'NONE',  ( 27.30736127486511577, 7.960716467858479639, -228.6121938484450595 ) ) ;
#4700 = CARTESIAN_POINT ( 'NONE',  ( 2.980115756258533644, -14.12936798750240008, -229.0659090661425807 ) ) ;
#4701 = DIRECTION ( 'NONE',  ( 0.000000000000000000, 0.000000000000000000, 1.000000000000000000 ) ) ;
#4702 = CARTESIAN_POINT ( 'NONE',  ( -31.76239872120898511, 5.177298019713663990, -226.5714959923072342 ) ) ;
#4703 = CARTESIAN_POINT ( 'NONE',  ( 12.92410717862594893, 29.37236178718849189, -224.5435071569520744 ) ) ;
#4704 = CARTESIAN_POINT ( 'NONE',  ( 3.764125772070460396, 11.78312483992801596, -228.3484643988637970 ) ) ;
#4705 = CARTESIAN_POINT ( 'NONE',  ( 22.30453140437255044, -8.121595866981794032, -232.1448055058014575 ) ) ;
#4706 = CARTESIAN_POINT ( 'NONE',  ( -11.42613629117093765, 28.09170287990588832, -228.7150250545069241 ) ) ;
#4707 = CARTESIAN_POINT ( 'NONE',  ( -15.15434969228324924, 4.423874646950748613, -230.6144467931089821 ) ) ;
#4708 = CARTESIAN_POINT ( 'NONE',  ( 14.75291830987536557, 13.43762972591284033, -235.1407057970265839 ) ) ;
#4709 = CARTESIAN_POINT ( 'NONE',  ( -15.23792247720107440, 7.806131751461257373, -230.3336101049160902 ) ) ;
#4710 = CARTESIAN_POINT ( 'NONE',  ( -11.69688825528096388, 18.63404371591177622, -215.8612738028812714 ) ) ;
#4711 = DIRECTION ( 'NONE',  ( 0.000000000000000000, 0.000000000000000000, -1.000000000000000000 ) ) ;
#4712 = CARTESIAN_POINT ( 'NONE',  ( 3.388180927852674884, 15.71154068801650538, -224.9339660840813053 ) ) ;
#4713 = CARTESIAN_POINT ( 'NONE',  ( 27.32546652195855685, -7.354568365469916991, -229.0866163655393279 ) ) ;
#4714 = DIRECTION ( 'NONE',  ( 0.000000000000000000, 0.000000000000000000, -1.000000000000000000 ) ) ;
#4715 = CARTESIAN_POINT ( 'NONE',  ( -23.14980455159086503, 0.3541108476526578785, -217.8785187302087536 ) ) ;
#4716 = CARTESIAN_POINT ( 'NONE',  ( 25.33562512631297281, 12.25422971834577268, -228.6777356031426791 ) ) ;
#4717 = CARTESIAN_POINT ( 'NONE',  ( -18.40842514464981861, -18.33793064768350334, -230.6214457472987931 ) ) ;
#4718 = CARTESIAN_POINT ( 'NONE',  ( 0.000000000000000000, 0.000000000000000000, 77.51594804401857175 ) ) ;
#4719 = CARTESIAN_POINT ( 'NONE',  ( -4.142636420702924482, 14.17169704882741321, -225.1666440184957310 ) ) ;
#4720 = SHAPE_REPRESENTATION_RELATIONSHIP ( 'NONE' , 'NONE' ,  #9901, #5876 ) ;
#4721 = CARTESIAN_POINT ( 'NONE',  ( 19.66153801111809685, -22.47763448259700780, -224.4992982350615023 ) ) ;
#4722 = ADVANCED_FACE ( 'NONE', ( #12882 ), #19732, .F. ) ;
#4723 = CARTESIAN_POINT ( 'NONE',  ( 10.49810582199713416, 9.357428619962972149, -224.5466107281195605 ) ) ;
#4724 = CARTESIAN_POINT ( 'NONE',  ( -4.170472558179216804, 16.67407401355319152, -230.2690496885289804 ) ) ;
#4725 = CARTESIAN_POINT ( 'NONE',  ( -13.17897211815351000, 23.48099580033777301, -217.3415693533541173 ) ) ;
#4726 = VERTEX_POINT ( 'NONE', #951 ) ;
#4727 = CARTESIAN_POINT ( 'NONE',  ( -14.91191843134457784, -11.59770670008449756, -219.5316993567479642 ) ) ;
#4728 = EDGE_CURVE ( 'NONE', #10662, #7309, #14691, .T. ) ;
#4729 = CARTESIAN_POINT ( 'NONE',  ( 13.85822045549773129, -1.469587484828172919, -226.8778453516271156 ) ) ;
#4730 = AXIS2_PLACEMENT_3D ( 'NONE', #16261, #19515, #4102 ) ;
#4731 = EDGE_CURVE ( 'NONE', #15638, #10545, #11213, .T. ) ;
#4732 = DIRECTION ( 'NONE',  ( -0.000000000000000000, -0.000000000000000000, 1.000000000000000000 ) ) ;
#4733 = CARTESIAN_POINT ( 'NONE',  ( -27.49927005802855717, -8.180762508579555004, -232.0193187950690970 ) ) ;
#4734 = CARTESIAN_POINT ( 'NONE',  ( 16.96779410054824666, 23.69881408353223406, -220.2174342377987841 ) ) ;
#4735 = CARTESIAN_POINT ( 'NONE',  ( -14.59766675578715223, 7.926254675926275972, -222.3706877972550444 ) ) ;
#4736 = CARTESIAN_POINT ( 'NONE',  ( 2.804048525646705148, 30.59371477727813726, -220.6614663749232363 ) ) ;
#4737 = CARTESIAN_POINT ( 'NONE',  ( 25.02650711521362936, 17.58144575069911042, -223.6165279156031431 ) ) ;
#4738 = ORIENTED_EDGE ( 'NONE', *, *, #19426, .T. ) ;
#4739 = CARTESIAN_POINT ( 'NONE',  ( -18.06397433365231819, -19.82544507610489859, -216.4780239895989951 ) ) ;
#4740 = ORIENTED_EDGE ( 'NONE', *, *, #18322, .F. ) ;
#4741 = CARTESIAN_POINT ( 'NONE',  ( -7.972347216402701164, -18.74702622849856937, -232.1058264431568148 ) ) ;
#4742 = CARTESIAN_POINT ( 'NONE',  ( -29.65068623107463708, 4.004319520977249525, -231.5200339834770773 ) ) ;
#4743 = CARTESIAN_POINT ( 'NONE',  ( 8.332496243628455090, -29.79192972398156769, -226.1452587264855367 ) ) ;
#4744 = CARTESIAN_POINT ( 'NONE',  ( -14.93108815068229589, -1.792787290847115633, -227.6165763581034582 ) ) ;
#4745 = CARTESIAN_POINT ( 'NONE',  ( -23.10791503177032880, -5.282985115830100220, -217.6364121950018671 ) ) ;
#4746 = CARTESIAN_POINT ( 'NONE',  ( 19.61276001257277102, 19.97122404150989894, -229.5162757829903342 ) ) ;
#4747 = CARTESIAN_POINT ( 'NONE',  ( 21.50000000000001066, 2.632990618166810813E-15, -65.00000000000000000 ) ) ;
#4748 = CARTESIAN_POINT ( 'NONE',  ( -14.64425879132321384, 10.88727730234500868, -217.2315376225554644 ) ) ;
#4749 = CARTESIAN_POINT ( 'NONE',  ( 12.79953165872901266, 10.20044330008568778, -230.3912386799665626 ) ) ;
#4750 = CARTESIAN_POINT ( 'NONE',  ( -1.249406995060579062, 25.48934319316224162, -216.9406480707515072 ) ) ;
#4751 = CARTESIAN_POINT ( 'NONE',  ( 8.645835506124264214, 12.38899589144949687, -223.4673650485651990 ) ) ;
#4752 = CARTESIAN_POINT ( 'NONE',  ( 9.191046577198441980, -13.34937224525895161, -233.4761082295262611 ) ) ;
#4753 = B_SPLINE_CURVE_WITH_KNOTS ( 'NONE', 3,
 ( #10771, #8978, #12237, #17637, #3450, #17299, #15842, #1874, #19088, #3664, #1769, #418, #10330, #10550, #17419, #8643, #17192, #15504, #20663, #5245, #12127, #3561, #18074, #9633, #13004, #7405, #965, #7616, #14484, #14705, #12792, #11102, #21539, #19850, #636, #14275, #21107, #2646, #6024, #12572, #12897, #21213, #7512, #12680, #2752, #14379, #16275, #4222, #11208, #5799 ),
 .UNSPECIFIED., .F., .F.,
 ( 4, 2, 2, 2, 2, 2, 2, 2, 2, 2, 2, 2, 2, 2, 2, 2, 2, 2, 2, 2, 2, 2, 2, 2, 4 ),
 ( 0.03166499401898992955, 0.03265355373879610251, 0.03364211345860227548, 0.03561923289821462141, 0.03660779261802078743, 0.03759635233782696040, 0.03858491205763313336, 0.03957347177743930633, 0.04155059121705165226, 0.04253915093685782522, 0.04352771065666399819, 0.04550483009627633718, 0.04649338981608251015, 0.04748194953588867617, 0.04945906897550102210, 0.05143618841511336803, 0.05341330785472571396, 0.05539042729433805989, 0.05637898701414422592, 0.05736754673395039889, 0.05835610645375657185, 0.05934466617356273788, 0.06132178561317508381, 0.06231034533298125677, 0.06329890505278742974 ),
 .UNSPECIFIED. ) ;
#4754 = CARTESIAN_POINT ( 'NONE',  ( -6.496078068315311427, 23.46891392553531119, -233.1042179568201220 ) ) ;
#4755 = CARTESIAN_POINT ( 'NONE',  ( -6.266309075335420253, -15.78290365675015572, -230.2363798222519051 ) ) ;
#4756 = CARTESIAN_POINT ( 'NONE',  ( -13.65925618638770800, 3.289586759644148817, -222.1579143493116533 ) ) ;
#4757 = CIRCLE ( 'NONE', #1171, 23.00000000000000000 ) ;
#4758 = CARTESIAN_POINT ( 'NONE',  ( 0.000000000000000000, 22.63401512838748175, -77.51594804401857175 ) ) ;
#4759 = AXIS2_PLACEMENT_3D ( 'NONE', #10909, #12825, #2679 ) ;
#4760 = CARTESIAN_POINT ( 'NONE',  ( 14.22574309452842733, 4.476723532073429546, -225.5862451792618231 ) ) ;
#4761 = CARTESIAN_POINT ( 'NONE',  ( 8.625046000483031605, -27.40455649025574303, -220.2318935480384710 ) ) ;
#4762 = CARTESIAN_POINT ( 'NONE',  ( -26.02492405343843984, 6.940268742526972900, -218.8798307745116460 ) ) ;
#4763 = CARTESIAN_POINT ( 'NONE',  ( 7.163080459435270164, 24.05253566895842354, -232.4475987112033408 ) ) ;
#4764 = CARTESIAN_POINT ( 'NONE',  ( -13.22951852716680676, -5.246159916193459338, -223.7538483380451453 ) ) ;
#4765 = CARTESIAN_POINT ( 'NONE',  ( 13.16746181015946959, 0.3897807143096829741, -227.1676274388083243 ) ) ;
#4766 = EDGE_CURVE ( 'NONE', #16533, #19761, #22097, .T. ) ;
#4767 = CARTESIAN_POINT ( 'NONE',  ( 12.65306858828212810, 29.42930486385247590, -226.3758484992818012 ) ) ;
#4768 = ORIENTED_EDGE ( 'NONE', *, *, #21373, .T. ) ;
#4769 = CARTESIAN_POINT ( 'NONE',  ( -3.673551555920188783, 29.81207051619892923, -228.8770490300152005 ) ) ;
#4770 = CARTESIAN_POINT ( 'NONE',  ( 13.21219219391003818, -8.064832675337259005, -225.0434479037668041 ) ) ;
#4771 = CARTESIAN_POINT ( 'NONE',  ( -24.24407467525207238, -6.106727297653192110, -7.925496382379915161 ) ) ;
#4772 = DIRECTION ( 'NONE',  ( 0.000000000000000000, 1.000000000000000000, -0.000000000000000000 ) ) ;
#4773 = CARTESIAN_POINT ( 'NONE',  ( 5.141746912158045468, 22.01688500372448232, -216.6678693612369386 ) ) ;
#4774 = CARTESIAN_POINT ( 'NONE',  ( -5.787689185779406387, -30.68964578337966387, -228.1462806397894383 ) ) ;
#4775 = CARTESIAN_POINT ( 'NONE',  ( 5.434900225474387447, -11.93567727083262042, -224.7511004068755369 ) ) ;
#4776 = AXIS2_PLACEMENT_3D ( 'NONE', #12920, #16411, #9331 ) ;
#4777 = CARTESIAN_POINT ( 'NONE',  ( 17.02763684969102798, -14.67205317233652195, -233.2001291093645818 ) ) ;
#4778 = AXIS2_PLACEMENT_3D ( 'NONE', #21318, #2203, #12679 ) ;
#4779 = CARTESIAN_POINT ( 'NONE',  ( -11.05707385098054729, 9.265475627845670914, -220.9763772784480693 ) ) ;
#4780 = CARTESIAN_POINT ( 'NONE',  ( 8.132753622789847370, 14.44084924206385701, -222.7013822740049704 ) ) ;
#4781 = DIRECTION ( 'NONE',  ( -0.000000000000000000, -0.000000000000000000, -1.000000000000000000 ) ) ;
#4782 = CARTESIAN_POINT ( 'NONE',  ( -22.57344584932824105, 14.14390280519600473, -217.2212543695777924 ) ) ;
#4783 = CARTESIAN_POINT ( 'NONE',  ( -14.27150057966913721, -8.785576370668652046, -221.5154223125717579 ) ) ;
#4784 = ORIENTED_EDGE ( 'NONE', *, *, #20402, .T. ) ;
#4785 = CARTESIAN_POINT ( 'NONE',  ( -16.50467377682197423, 21.56569464670658220, -229.9175202103629374 ) ) ;
#4786 = CARTESIAN_POINT ( 'NONE',  ( 23.22505041959077232, 19.39625294115234055, -221.5972645870541555 ) ) ;
#4787 = CARTESIAN_POINT ( 'NONE',  ( 1.682843645364419993, 12.02583837823347679, -224.9288196625490457 ) ) ;
#4788 = CARTESIAN_POINT ( 'NONE',  ( 14.58943670538545412, -3.864781073802256550, -230.4050158740328129 ) ) ;
#4789 = DIRECTION ( 'NONE',  ( 1.000000000000000000, 0.000000000000000000, 0.000000000000000000 ) ) ;
#4790 = ORIENTED_EDGE ( 'NONE', *, *, #20520, .F. ) ;
#4791 = CARTESIAN_POINT ( 'NONE',  ( -28.13472254077564116, 12.33996625515159629, -224.9141344439281909 ) ) ;
#4792 = CARTESIAN_POINT ( 'NONE',  ( -30.36433721104044992, -10.30696067327809651, -227.5875578433412159 ) ) ;
#4793 = DIRECTION ( 'NONE',  ( 0.000000000000000000, 1.000000000000000000, 0.000000000000000000 ) ) ;
#4794 = CARTESIAN_POINT ( 'NONE',  ( 18.23324537670537993, 23.47692953258263771, -224.8333321331434433 ) ) ;
#4795 = DIRECTION ( 'NONE',  ( -1.000000000000000000, 0.000000000000000000, 0.000000000000000000 ) ) ;
#4796 = AXIS2_PLACEMENT_3D ( 'NONE', #6724, #5020, #1207 ) ;
#4797 = VECTOR ( 'NONE', #2097, 1000.000000000000000 ) ;
#4798 = CARTESIAN_POINT ( 'NONE',  ( 12.31511859722645852, -8.491226738247512174, -220.9006323875693738 ) ) ;
#4799 = CARTESIAN_POINT ( 'NONE',  ( -13.69675006931110417, 3.702342960760605539, -228.0723273272095355 ) ) ;
#4800 = CARTESIAN_POINT ( 'NONE',  ( -19.90771709537278156, 23.83218599423810602, -225.0439263757368735 ) ) ;
#4801 = CARTESIAN_POINT ( 'NONE',  ( 15.18181359483165949, 6.369295616116027681, -230.7949408486033462 ) ) ;
#4802 =( NAMED_UNIT ( * ) SI_UNIT ( $, .STERADIAN. ) SOLID_ANGLE_UNIT ( ) );
#4803 = CARTESIAN_POINT ( 'NONE',  ( -24.04585643156664077, 6.844992825942523673, -7.297348454157751796 ) ) ;
#4804 = CARTESIAN_POINT ( 'NONE',  ( 28.57344184061583192, 5.631897254180425527, -225.1192013637692355 ) ) ;
#4805 = CARTESIAN_POINT ( 'NONE',  ( -23.00000000000000000, 0.000000000000000000, -30.00000000000000000 ) ) ;
#4806 = CARTESIAN_POINT ( 'NONE',  ( 27.35305420947085153, -2.513179086165481912, -228.1718430395816881 ) ) ;
#4807 = CARTESIAN_POINT ( 'NONE',  ( -15.19144047750087267, -10.24270553329939304, -232.4311702607364793 ) ) ;
#4808 = DIRECTION ( 'NONE',  ( -0.000000000000000000, -0.000000000000000000, 1.000000000000000000 ) ) ;
#4809 = PLANE ( 'NONE',  #1899 ) ;
#4810 = CARTESIAN_POINT ( 'NONE',  ( 0.3355639943343493026, 23.87279439325363128, -218.0067922387550823 ) ) ;
#4811 = CARTESIAN_POINT ( 'NONE',  ( 6.264370104348762069, -18.85623240742893714, -216.4903287596617076 ) ) ;
#4812 = CARTESIAN_POINT ( 'NONE',  ( 13.36656406724190305, -19.73987914515934960, -233.3798509643240209 ) ) ;
#4813 = ORIENTED_EDGE ( 'NONE', *, *, #5651, .T. ) ;
#4814 = CARTESIAN_POINT ( 'NONE',  ( -17.14223598032838325, 23.31797360549976261, -226.5771676936548431 ) ) ;
#4815 = CARTESIAN_POINT ( 'NONE',  ( -15.99768154740552717, 2.245235659047613908, -226.7015216759272107 ) ) ;
#4816 = CARTESIAN_POINT ( 'NONE',  ( 25.18311526135610734, 13.65721788432563955, -224.7326014392022273 ) ) ;
#4817 = EDGE_LOOP ( 'NONE', ( #6352, #1844, #564, #21444 ) ) ;
#4818 = CIRCLE ( 'NONE', #9908, 2.999999999999999112 ) ;
#4819 = CARTESIAN_POINT ( 'NONE',  ( -8.126933673790581736, -26.89509779614531126, -227.4795931708183048 ) ) ;
#4820 = CARTESIAN_POINT ( 'NONE',  ( -8.055668064929562888, -7.157650466794454935, 91.99999999999997158 ) ) ;
#4821 = CARTESIAN_POINT ( 'NONE',  ( -29.65068623107463708, 4.004319520977249525, -231.5200339834770773 ) ) ;
#4822 = CARTESIAN_POINT ( 'NONE',  ( 10.61539692146153691, 8.157890242340682718, -227.5705019877536301 ) ) ;
#4823 = CARTESIAN_POINT ( 'NONE',  ( 29.72361553920624999, -4.223772423702004453, -224.3921473884441866 ) ) ;
#4824 = CARTESIAN_POINT ( 'NONE',  ( 0.9908753270255351575, 13.79205759140780430, -228.0165926715089881 ) ) ;
#4825 = CARTESIAN_POINT ( 'NONE',  ( -27.29953305526601426, 11.21644211419729054, -229.3676346105362995 ) ) ;
#4826 = CARTESIAN_POINT ( 'NONE',  ( 10.00603923119254723, 9.610873433734882454, -231.2388095806506669 ) ) ;
#4827 = CARTESIAN_POINT ( 'NONE',  ( -25.48569860171343748, 4.299098795181173216, -219.7804659532078801 ) ) ;
#4828 = APPLICATION_CONTEXT ( 'automotive_design' ) ;
#4829 = CARTESIAN_POINT ( 'NONE',  ( -15.66530208164916260, 23.23467148471576849, -218.1250122661128046 ) ) ;
#4830 = AXIS2_PLACEMENT_3D ( 'NONE', #2286, #607, #1127 ) ;
#4831 = CARTESIAN_POINT ( 'NONE',  ( 4.782033626261160464, 9.864562363145058299, 92.00000000000000000 ) ) ;
#4832 = CARTESIAN_POINT ( 'NONE',  ( 3.241594727517011609, 27.64703009302456138, -225.5540025036233374 ) ) ;
#4833 = CARTESIAN_POINT ( 'NONE',  ( 20.80196158924851701, -7.261721507697286526, -217.3074963141844194 ) ) ;
#4834 = CARTESIAN_POINT ( 'NONE',  ( 0.000000000000000000, 0.000000000000000000, -75.00000000000000000 ) ) ;
#4835 = CARTESIAN_POINT ( 'NONE',  ( -18.34948365288241590, -1.907751280579004893, -231.5848060246952116 ) ) ;
#4836 = CARTESIAN_POINT ( 'NONE',  ( -14.74212732455322161, 0.2624230007780231633, -231.8143822214177874 ) ) ;
#4837 = CARTESIAN_POINT ( 'NONE',  ( -11.81856518996410088, -14.35937779267807279, -219.1576658967449305 ) ) ;
#4838 = CARTESIAN_POINT ( 'NONE',  ( 0.000000000000000000, 0.000000000000000000, -30.00000000000000000 ) ) ;
#4839 = CARTESIAN_POINT ( 'NONE',  ( -4.334015487506815312, 18.19775486192265390, -231.4387392399519285 ) ) ;
#4840 =( NAMED_UNIT ( * ) SI_UNIT ( $, .STERADIAN. ) SOLID_ANGLE_UNIT ( ) );
#4841 = CARTESIAN_POINT ( 'NONE',  ( 5.191785474240024456, -25.78595846473334419, -219.2330600099714673 ) ) ;
#4842 = CARTESIAN_POINT ( 'NONE',  ( 13.88312867625433711, 12.44451767566605760, -217.7066242262208391 ) ) ;
#4843 = CARTESIAN_POINT ( 'NONE',  ( -6.720912670637915198, 19.69156892798266512, -217.8848069150180891 ) ) ;
#4844 = CARTESIAN_POINT ( 'NONE',  ( -7.686214453470440411, 10.71593237010305444, -228.8058998235944159 ) ) ;
#4845 = ORIENTED_EDGE ( 'NONE', *, *, #5629, .T. ) ;
#4846 = CARTESIAN_POINT ( 'NONE',  ( -27.21693968233852701, -2.213369147249347524, -221.9579181326467392 ) ) ;
#4847 = CARTESIAN_POINT ( 'NONE',  ( 17.19674704922021391, 23.07334190050143974, -228.8256488842130238 ) ) ;
#4848 = EDGE_CURVE ( 'NONE', #1422, #18158, #15892, .T. ) ;
#4849 = CARTESIAN_POINT ( 'NONE',  ( 14.95834318372430083, -1.617016552789838801, -229.6306532055809271 ) ) ;
#4850 = AXIS2_PLACEMENT_3D ( 'NONE', #19232, #3812, #7433 ) ;
#4851 = DIRECTION ( 'NONE',  ( 0.000000000000000000, 0.000000000000000000, -1.000000000000000000 ) ) ;
#4852 = CARTESIAN_POINT ( 'NONE',  ( 26.16486877413895584, -0.2437668799822691745, -230.8325409000573814 ) ) ;
#4853 = CARTESIAN_POINT ( 'NONE',  ( 10.49811526528768368, 13.26166588535847701, -217.9009921269571919 ) ) ;
#4854 = CARTESIAN_POINT ( 'NONE',  ( -14.20363567091065349, 7.857660128015216294, -223.4151327167956822 ) ) ;
#4855 = CARTESIAN_POINT ( 'NONE',  ( 0.8673818989965740300, 28.69424263383094598, -231.7310846804014659 ) ) ;
#4856 = EDGE_CURVE ( 'NONE', #16533, #14290, #1856, .T. ) ;
#4857 = CARTESIAN_POINT ( 'NONE',  ( 15.21408433160105034, 3.021350230896802103, -222.3056493717910769 ) ) ;
#4858 = EDGE_LOOP ( 'NONE', ( #20308, #6148, #21779, #21619, #19846, #15828 ) ) ;
#4859 = CARTESIAN_POINT ( 'NONE',  ( -13.74974073587016576, -14.61773948691506142, -215.3128624239759290 ) ) ;
#4860 = ORIENTED_EDGE ( 'NONE', *, *, #5761, .F. ) ;
#4861 = CARTESIAN_POINT ( 'NONE',  ( -11.82217545354207644, -11.78227988727524966, -219.0934395369134506 ) ) ;
#4862 = CARTESIAN_POINT ( 'NONE',  ( -16.99821283087967672, -0.5135051709387361552, -216.2173766440975555 ) ) ;
#4863 = CARTESIAN_POINT ( 'NONE',  ( 5.668262076144046979, -25.28042871382391965, -216.8182873783340483 ) ) ;
#4864 = CARTESIAN_POINT ( 'NONE',  ( 13.34086609499694553, -4.728578536804411314, -230.1381470621469134 ) ) ;
#4865 = CARTESIAN_POINT ( 'NONE',  ( -22.53818779203657741, -7.663114047788936567, -232.6164956747681458 ) ) ;
#4866 = AXIS2_PLACEMENT_3D ( 'NONE', #11626, #13095, #12979 ) ;
#4867 = CARTESIAN_POINT ( 'NONE',  ( 13.17768061945195157, 6.810183613937965674, -219.8302315341053657 ) ) ;
#4868 = CARTESIAN_POINT ( 'NONE',  ( -27.05172747931452903, 14.36075930490012276, -228.5082213655825853 ) ) ;
#4869 = CARTESIAN_POINT ( 'NONE',  ( 20.40268796714816801, 18.65534563792085621, -219.5587498978784993 ) ) ;
#4870 = CARTESIAN_POINT ( 'NONE',  ( 10.55627441269396094, 10.31758739525044888, -223.1990319438957613 ) ) ;
#4871 = CARTESIAN_POINT ( 'NONE',  ( 8.812670488384366507, 12.21486833790445914, -225.9961634525829197 ) ) ;
#4872 = CARTESIAN_POINT ( 'NONE',  ( 25.51806929334465934, -15.64550748320022144, -218.8629450469393589 ) ) ;
#4873 = CARTESIAN_POINT ( 'NONE',  ( -10.65640919150578192, 23.79238421564942740, -218.1088542024188826 ) ) ;
#4874 = CARTESIAN_POINT ( 'NONE',  ( -24.68906941503829700, 2.445024713909649705, -232.6803430500543755 ) ) ;
#4875 = DIRECTION ( 'NONE',  ( -0.9940043559354330149, -0.1093404791528966163, -6.737719923507020479E-14 ) ) ;
#4876 = CARTESIAN_POINT ( 'NONE',  ( 15.33737796850231305, 13.57479350230705428, -232.3313557812109025 ) ) ;
#4877 = CARTESIAN_POINT ( 'NONE',  ( 14.99967020447171784, -24.16696097797641940, -221.8072564961694297 ) ) ;
#4878 = CARTESIAN_POINT ( 'NONE',  ( -12.43544732248594720, 12.69828336922617318, -219.3367909706387877 ) ) ;
#4879 = AXIS2_PLACEMENT_3D ( 'NONE', #12519, #1819, #14328 ) ;
#4880 = CARTESIAN_POINT ( 'NONE',  ( 5.955271202636533090, 21.50135983300913267, -233.0184468368920534 ) ) ;
#4881 = CARTESIAN_POINT ( 'NONE',  ( -20.18470553695442860, -13.13924840112635195, -232.9662461559857718 ) ) ;
#4882 = CARTESIAN_POINT ( 'NONE',  ( -26.87016840655871874, 6.086699737350822481, -222.9228935003981746 ) ) ;
#4883 = CARTESIAN_POINT ( 'NONE',  ( 8.454338299486085617, 13.28844197278511530, -217.6979371188311632 ) ) ;
#4884 = ORIENTED_EDGE ( 'NONE', *, *, #7094, .F. ) ;
#4885 = CARTESIAN_POINT ( 'NONE',  ( 0.9046320824004248085, 13.39785254849979701, -226.4815711199935890 ) ) ;
#4886 = CARTESIAN_POINT ( 'NONE',  ( 11.63667859525082093, -10.90089931597979600, -224.9413544669828013 ) ) ;
#4887 = CARTESIAN_POINT ( 'NONE',  ( 18.43413881788024611, -3.292634616013774274, -216.7808090690139409 ) ) ;
#4888 = CARTESIAN_POINT ( 'NONE',  ( -6.938893903907228378E-15, 0.000000000000000000, -224.9999999999999716 ) ) ;
#4889 = CARTESIAN_POINT ( 'NONE',  ( 5.169766346882679997, 29.28517558595074988, -221.5178724947562614 ) ) ;
#4890 = CARTESIAN_POINT ( 'NONE',  ( -15.25474278246548643, -4.999135024540048988, -232.7276810733381183 ) ) ;
#4891 = CARTESIAN_POINT ( 'NONE',  ( -12.11864581566431553, -23.10742878804749978, -232.9192999331436909 ) ) ;
#4892 = CARTESIAN_POINT ( 'NONE',  ( 15.60497028854143764, -26.39208911975253002, -225.8550158017044112 ) ) ;
#4893 = CARTESIAN_POINT ( 'NONE',  ( -14.98215928292561294, 22.79623052288931362, -230.3289734367122890 ) ) ;
#4894 = CARTESIAN_POINT ( 'NONE',  ( 9.132190541728901323, 17.73033835127231939, -219.5524510795130766 ) ) ;
#4895 = CARTESIAN_POINT ( 'NONE',  ( -13.10651848559790444, 3.262242204071156948, -224.3513854875720597 ) ) ;
#4896 = CARTESIAN_POINT ( 'NONE',  ( -20.80338291456855870, 18.97067006663518995, -230.9007617602332516 ) ) ;
#4897 = CARTESIAN_POINT ( 'NONE',  ( -22.39763175122653038, -14.70415172796113623, -221.0757120432126612 ) ) ;
#4898 = AXIS2_PLACEMENT_3D ( 'NONE', #4718, #11489, #2918 ) ;
#4899 = ORIENTED_EDGE ( 'NONE', *, *, #11585, .F. ) ;
#4900 = CARTESIAN_POINT ( 'NONE',  ( -4.879985665934096772, 15.33285679834440174, -220.9402849574511833 ) ) ;
#4901 = CARTESIAN_POINT ( 'NONE',  ( 15.91624278015930649, 5.932232821383347954, -217.3600859879243217 ) ) ;
#4902 = CARTESIAN_POINT ( 'NONE',  ( 18.99256614858759207, 26.22894869843687715, -224.5811130452664202 ) ) ;
#4903 = CARTESIAN_POINT ( 'NONE',  ( 13.93061470302797389, -11.80544459979379646, -217.9389246709861538 ) ) ;
#4904 = CARTESIAN_POINT ( 'NONE',  ( 1.526556658859590496E-13, -21.80000000000006111, 78.50000000000000000 ) ) ;
#4905 = EDGE_LOOP ( 'NONE', ( #17625, #7710, #13023, #7597, #9429, #18268 ) ) ;
#4906 = CARTESIAN_POINT ( 'NONE',  ( -19.25929423112888017, 9.818144317380269825, -216.1837936240308409 ) ) ;
#4907 = CARTESIAN_POINT ( 'NONE',  ( -11.89542047990565266, -6.454581786823162304, -219.2692666839191133 ) ) ;
#4908 = LINE ( 'NONE', #15393, #12641 ) ;
#4909 = CARTESIAN_POINT ( 'NONE',  ( 13.61707622192329481, 14.84143455326118932, -217.6958999636067063 ) ) ;
#4910 = CYLINDRICAL_SURFACE ( 'NONE', #5521, 23.00000000000008882 ) ;
#4911 = CARTESIAN_POINT ( 'NONE',  ( 14.34945462593695531, -6.128426910066905542, -229.1128190117150041 ) ) ;
#4912 =( LENGTH_UNIT ( ) NAMED_UNIT ( * ) SI_UNIT ( .MILLI., .METRE. ) );
#4913 = CARTESIAN_POINT ( 'NONE',  ( -14.68037037322036475, 3.441677802729143920, -220.1396515630443389 ) ) ;
#4914 = PRODUCT_DEFINITION_SHAPE ( 'NONE', 'NONE',  #14016 ) ;
#4915 = ADVANCED_FACE ( 'NONE', ( #17343 ), #13439, .F. ) ;
#4916 = CARTESIAN_POINT ( 'NONE',  ( -7.812160407601123069, 10.19183344000749081, -223.8148904943605828 ) ) ;
#4917 = CARTESIAN_POINT ( 'NONE',  ( 15.92396645628901020, -0.3225394686005420009, -223.0199929375764327 ) ) ;
#4918 = CARTESIAN_POINT ( 'NONE',  ( -13.29422863469367577, -26.11207831950312652, -226.3284374130324750 ) ) ;
#4919 = DIRECTION ( 'NONE',  ( 0.000000000000000000, 0.000000000000000000, -1.000000000000000000 ) ) ;
#4920 = CARTESIAN_POINT ( 'NONE',  ( 24.58316096239279602, 5.861425670879941485, -231.3104446318280623 ) ) ;
#4921 = DIRECTION ( 'NONE',  ( -1.000000000000000000, 0.000000000000000000, 0.000000000000000000 ) ) ;
#4922 = CARTESIAN_POINT ( 'NONE',  ( 14.64841443880303373, -15.14843974207636101, -218.3573740752273125 ) ) ;
#4923 = CARTESIAN_POINT ( 'NONE',  ( 12.84273949316563801, -2.956482729363947737, -224.4564014745444638 ) ) ;
#4924 = CARTESIAN_POINT ( 'NONE',  ( -21.17788351146302617, -8.976196367870899806, -4.455375687320114686 ) ) ;
#4925 = CARTESIAN_POINT ( 'NONE',  ( 9.653903571287008489, 19.16609876806546353, -219.1149796918802792 ) ) ;
#4926 = CARTESIAN_POINT ( 'NONE',  ( 20.78003164828882632, -23.67023879211220461, -227.8573985392403074 ) ) ;
#4927 = CARTESIAN_POINT ( 'NONE',  ( 9.918856707546316542, -11.48950767347732871, -219.9734948840342668 ) ) ;
#4928 = EDGE_LOOP ( 'NONE', ( #14011, #17456, #18782, #21763 ) ) ;
#4929 = CARTESIAN_POINT ( 'NONE',  ( -10.29720673141181209, 11.14783905173092649, -222.8560683878917530 ) ) ;
#4930 = CARTESIAN_POINT ( 'NONE',  ( 14.00715608756928532, 4.299235856235253728, -230.2440235370780215 ) ) ;
#4931 = CARTESIAN_POINT ( 'NONE',  ( 20.64430047260004031, 12.67811357335941480, -231.0449411089858813 ) ) ;
#4932 = VERTEX_POINT ( 'NONE', #19024 ) ;
#4933 = CARTESIAN_POINT ( 'NONE',  ( -3.424405916006480144, -18.03457810294644403, -219.2650390415759318 ) ) ;
#4934 = CARTESIAN_POINT ( 'NONE',  ( 7.485089409085513346, -7.743278074783935594, 91.99999999999998579 ) ) ;
#4935 = CARTESIAN_POINT ( 'NONE',  ( -14.70339349403010942, -0.4153334646997780544, -217.8790668391084466 ) ) ;
#4936 = CARTESIAN_POINT ( 'NONE',  ( 9.851209273476317918, 25.48401176094959553, -233.7173763849377792 ) ) ;
#4937 = CARTESIAN_POINT ( 'NONE',  ( 10.85023464552735462, -16.86364573545779777, -230.5238403791007045 ) ) ;
#4938 = CARTESIAN_POINT ( 'NONE',  ( 12.18657022793382794, 26.76558097653315471, -221.8882195427397335 ) ) ;
#4939 = CARTESIAN_POINT ( 'NONE',  ( -19.25929423112888017, 9.818144317380269825, -216.1837936240308409 ) ) ;
#4940 = EDGE_CURVE ( 'NONE', #215, #21209, #15525, .T. ) ;
#4941 = CARTESIAN_POINT ( 'NONE',  ( 10.86206282953156510, 30.27427353967719981, -226.0953027964478110 ) ) ;
#4942 = CARTESIAN_POINT ( 'NONE',  ( -25.19195624009214640, 10.50676406307063182, -220.0954552869889937 ) ) ;
#4943 = CARTESIAN_POINT ( 'NONE',  ( -3.643097910890548796, 22.16888955197135047, -233.9701981029593298 ) ) ;
#4944 = CARTESIAN_POINT ( 'NONE',  ( 9.223872243966841467, 5.696734612111038487, 92.00000000000001421 ) ) ;
#4945 = CARTESIAN_POINT ( 'NONE',  ( 1.127544764349826867, -27.89617517048659323, -231.9509945439240823 ) ) ;
#4946 = CARTESIAN_POINT ( 'NONE',  ( 25.54997870115619207, -2.097555195297153841, -218.7002440566220400 ) ) ;
#4947 = CARTESIAN_POINT ( 'NONE',  ( 0.000000000000000000, 17.50000000000000711, -60.00000000000000000 ) ) ;
#4948 = DIRECTION ( 'NONE',  ( 0.000000000000000000, 0.000000000000000000, 1.000000000000000000 ) ) ;
#4949 = CARTESIAN_POINT ( 'NONE',  ( 25.18785298611088308, 3.974282393449815931, -218.7636041058819956 ) ) ;
#4950 = CARTESIAN_POINT ( 'NONE',  ( -16.08069336251900339, -10.46797077187589231, -230.6200287382480383 ) ) ;
#4951 = DIRECTION ( 'NONE',  ( -0.000000000000000000, -0.000000000000000000, 1.000000000000000000 ) ) ;
#4952 = CARTESIAN_POINT ( 'NONE',  ( 1.525817648051120967, -14.82969601928396841, -225.8796824437346515 ) ) ;
#4953 = CARTESIAN_POINT ( 'NONE',  ( 19.61276001257277102, 19.97122404150989894, -229.5162757829903342 ) ) ;
#4954 = CARTESIAN_POINT ( 'NONE',  ( -4.583529401292260275, 28.77615850237956607, -226.7744741901706504 ) ) ;
#4955 = CARTESIAN_POINT ( 'NONE',  ( -6.331039912586185814, 17.62337457105953220, -233.2305561356360499 ) ) ;
#4956 = CARTESIAN_POINT ( 'NONE',  ( -18.09422283036245460, -3.216155923901089064, -229.6485988878351918 ) ) ;
#4957 = ORIENTED_EDGE ( 'NONE', *, *, #9109, .F. ) ;
#4958 = CARTESIAN_POINT ( 'NONE',  ( 17.60676319847677007, 21.31475060840986302, -219.8266339603936785 ) ) ;
#4959 = CARTESIAN_POINT ( 'NONE',  ( -15.94549496081242346, -0.04271059606100771622, -224.7066567765017169 ) ) ;
#4960 = CARTESIAN_POINT ( 'NONE',  ( -18.94444594796027914, 3.458349568010113728, -218.9807021659310635 ) ) ;
#4961 = LINE ( 'NONE', #1807, #3698 ) ;
#4962 = EDGE_CURVE ( 'NONE', #1959, #18650, #20526, .T. ) ;
#4963 = CARTESIAN_POINT ( 'NONE',  ( -13.58432508418311180, -0.3977623232610293935, -228.1278904906119465 ) ) ;
#4964 = CARTESIAN_POINT ( 'NONE',  ( 16.10596270516584028, 24.75152718569329835, -228.9330127594856492 ) ) ;
#4965 = CARTESIAN_POINT ( 'NONE',  ( -14.01525440049806193, 8.239250543314939890, -226.5804714421811070 ) ) ;
#4966 = CARTESIAN_POINT ( 'NONE',  ( 9.400341091271927851, 28.64465517894215196, -231.0823126271420165 ) ) ;
#4967 = CARTESIAN_POINT ( 'NONE',  ( 25.70381634773192658, 10.55338509461953400, -230.3576492130207782 ) ) ;
#4968 = EDGE_CURVE ( 'NONE', #8552, #8796, #7346, .T. ) ;
#4969 = CARTESIAN_POINT ( 'NONE',  ( -19.52111408301234974, -15.33805657151784985, -234.6553009392178808 ) ) ;
#4970 = ORIENTED_EDGE ( 'NONE', *, *, #17531, .T. ) ;
#4971 = CARTESIAN_POINT ( 'NONE',  ( -11.24961133108761935, -10.18645864713539950, -228.7780882195199013 ) ) ;
#4972 = TOROIDAL_SURFACE ( 'NONE', #17574, 22.63401512838748175, 3.000000000000002665 ) ;
#4973 = CARTESIAN_POINT ( 'NONE',  ( -17.58289524052909414, 0.7988212499981205417, -233.9567931471624149 ) ) ;
#4974 = CARTESIAN_POINT ( 'NONE',  ( 15.65513449100897780, -26.00057195821942457, -227.4103383097017570 ) ) ;
#4975 = CARTESIAN_POINT ( 'NONE',  ( -3.060450601941519189, 13.29454208326677289, -222.0135664617158682 ) ) ;
#4976 = CARTESIAN_POINT ( 'NONE',  ( 16.37256825621668099, -5.086412116083368851, -216.7246661941694867 ) ) ;
#4977 = CARTESIAN_POINT ( 'NONE',  ( -26.43144772945995413, -6.745116643720071359, -219.5134289301136050 ) ) ;
#4978 = CARTESIAN_POINT ( 'NONE',  ( 12.54860906168727652, 6.077542143275485031, -228.1605930327268368 ) ) ;
#4979 = DIRECTION ( 'NONE',  ( 0.000000000000000000, 0.000000000000000000, 1.000000000000000000 ) ) ;
#4980 = CARTESIAN_POINT ( 'NONE',  ( -25.98311979368102342, 15.13734258059737670, -220.6162231662327429 ) ) ;
#4981 = CARTESIAN_POINT ( 'NONE',  ( 11.54460987479198053, 9.649171130674412566, -228.7280371210653698 ) ) ;
#4982 = CARTESIAN_POINT ( 'NONE',  ( 16.54345861550681107, 19.37554510112122230, -218.2240151908141002 ) ) ;
#4983 = CARTESIAN_POINT ( 'NONE',  ( 6.225744896574323839, 14.38227537199079720, -224.8391693295998266 ) ) ;
#4984 = CARTESIAN_POINT ( 'NONE',  ( -1.453954827973251929, -30.77017545459721859, -228.2950292831040713 ) ) ;
#4985 = CARTESIAN_POINT ( 'NONE',  ( -5.727886109716582297, 15.25217619989539486, -230.5419623196804650 ) ) ;
#4986 = CARTESIAN_POINT ( 'NONE',  ( 15.61962121506769385, 4.525360868525488911, -229.0684696061408090 ) ) ;
#4987 = CARTESIAN_POINT ( 'NONE',  ( 3.671249956548685578, -18.86103685443826805, -233.0640024924723548 ) ) ;
#4988 = CARTESIAN_POINT ( 'NONE',  ( -18.04772061096520375, 5.916925414182395038, -217.8829197293425750 ) ) ;
#4989 = CARTESIAN_POINT ( 'NONE',  ( 3.846342036506673612, 16.55327908958690131, -231.1358846258000597 ) ) ;
#4990 = CARTESIAN_POINT ( 'NONE',  ( -18.89430729770302975, -12.42271633246521212, -233.2230176520695295 ) ) ;
#4991 = CARTESIAN_POINT ( 'NONE',  ( 26.28575214971901630, 3.591103948354015696, -217.0994821834097763 ) ) ;
#4992 = CARTESIAN_POINT ( 'NONE',  ( 10.81638188557560731, 14.98959006186633403, -234.2424515599453514 ) ) ;
#4993 = ORIENTED_EDGE ( 'NONE', *, *, #12242, .T. ) ;
#4994 = CARTESIAN_POINT ( 'NONE',  ( -10.24288955603410933, 28.30762631303078791, -220.8855665231519083 ) ) ;
#4995 = CARTESIAN_POINT ( 'NONE',  ( 14.09645999499448088, -9.025099991742237648, -228.8994629750086744 ) ) ;
#4996 = CARTESIAN_POINT ( 'NONE',  ( 12.85536293311005451, -7.423602990911125410, -229.4216632760384300 ) ) ;
#4997 = DIRECTION ( 'NONE',  ( 0.000000000000000000, 0.000000000000000000, 1.000000000000000000 ) ) ;
#4998 = CARTESIAN_POINT ( 'NONE',  ( 12.04687593227112430, 27.54339840196571743, -224.6466266724203820 ) ) ;
#4999 = CARTESIAN_POINT ( 'NONE',  ( -14.02432777873800518, -4.625777501976016559, -231.5673840409723709 ) ) ;
#5000 = CARTESIAN_POINT ( 'NONE',  ( -7.531388159411753769, -21.98719092781708540, -216.0713624712111312 ) ) ;
#5001 = CARTESIAN_POINT ( 'NONE',  ( 7.021536848793814123, -14.49751826649810482, -218.4909385705359455 ) ) ;
#5002 = CARTESIAN_POINT ( 'NONE',  ( -21.95649697515285581, 20.70968357470995258, -226.9638023349746447 ) ) ;
#5003 = CARTESIAN_POINT ( 'NONE',  ( 10.73846460100926592, 12.62787417135106161, -222.6344468496098159 ) ) ;
#5004 = CARTESIAN_POINT ( 'NONE',  ( -23.98802705797876200, 19.46654170242919690, -223.5293093576406989 ) ) ;
#5005 = CARTESIAN_POINT ( 'NONE',  ( -22.28357709049062407, 7.264818440526320309, -215.3877468064711707 ) ) ;
#5006 = CARTESIAN_POINT ( 'NONE',  ( -17.40151406155100844, -6.170051014037699844, -218.8120118016391871 ) ) ;
#5007 = EDGE_LOOP ( 'NONE', ( #11084, #5257, #4307, #6425 ) ) ;
#5008 = CARTESIAN_POINT ( 'NONE',  ( -4.224287562409271501, 29.03635716824519264, -224.1823526280761882 ) ) ;
#5009 = CARTESIAN_POINT ( 'NONE',  ( 24.19635128940818447, 10.31396593861802380, -216.9479509989864425 ) ) ;
#5010 = CARTESIAN_POINT ( 'NONE',  ( 9.616550234602936342, 9.263684773868845923, -230.4827401731016607 ) ) ;
#5011 = ADVANCED_FACE ( 'NONE', ( #7965 ), #14725, .T. ) ;
#5012 = CARTESIAN_POINT ( 'NONE',  ( 13.20312407767240614, -7.650902547765872086, -230.0578600405493717 ) ) ;
#5013 = FACE_OUTER_BOUND ( 'NONE', #11808, .T. ) ;
#5014 = VERTEX_POINT ( 'NONE', #761 ) ;
#5015 = CARTESIAN_POINT ( 'NONE',  ( -3.368164009525018265, 19.03203264544105622, -233.5986411977714567 ) ) ;
#5016 = ADVANCED_FACE ( 'NONE', ( #8082 ), #9066, .T. ) ;
#5017 = CARTESIAN_POINT ( 'NONE',  ( -27.99742768613627319, -7.906662303124995184, -217.4094589651611216 ) ) ;
#5018 = FACE_OUTER_BOUND ( 'NONE', #18314, .T. ) ;
#5019 = CARTESIAN_POINT ( 'NONE',  ( 26.24002132888527328, 11.62331517472360964, -222.5300873157218859 ) ) ;
#5020 = DIRECTION ( 'NONE',  ( 0.000000000000000000, 0.000000000000000000, 1.000000000000000000 ) ) ;
#5021 = CARTESIAN_POINT ( 'NONE',  ( 13.04434844185555420, -10.19049307777131297, -230.8679447648462713 ) ) ;
#5022 = CARTESIAN_POINT ( 'NONE',  ( -14.07917727715460821, 7.534853284453274291, -218.6337090155677458 ) ) ;
#5023 = CARTESIAN_POINT ( 'NONE',  ( 26.53121369294028042, 10.74560293343441586, -229.2288136770759195 ) ) ;
#5024 = CARTESIAN_POINT ( 'NONE',  ( -1.827935560680505445, -14.81092009092713369, -225.7372845858837707 ) ) ;
#5025 = DIRECTION ( 'NONE',  ( -0.000000000000000000, -0.000000000000000000, 1.000000000000000000 ) ) ;
#5026 = CARTESIAN_POINT ( 'NONE',  ( 17.34727976380017722, 4.822939981779328811, -230.8836217450937909 ) ) ;
#5027 = LINE ( 'NONE', #13257, #16328 ) ;
#5028 = CARTESIAN_POINT ( 'NONE',  ( 15.55571562362403704, -22.93410568583619025, -228.9591035895856805 ) ) ;
#5029 = CARTESIAN_POINT ( 'NONE',  ( -1.232595164407830946E-29, 17.50000000000007105, -60.00000000000000000 ) ) ;
#5030 = CARTESIAN_POINT ( 'NONE',  ( 20.29114891157122358, -1.643118446426441892, -227.5163857825534421 ) ) ;
#5031 = CARTESIAN_POINT ( 'NONE',  ( 13.96918721733258195, 14.12724320058294403, -230.4946432816737172 ) ) ;
#5032 = CARTESIAN_POINT ( 'NONE',  ( 4.482815116226093188, 26.97722808566452812, -229.2080185206130238 ) ) ;
#5033 = CARTESIAN_POINT ( 'NONE',  ( 7.797975340826715396, -14.61189063385648623, -232.7894517818505733 ) ) ;
#5034 = CARTESIAN_POINT ( 'NONE',  ( 16.07085865561684201, -17.65509622858733252, -216.6880805489183501 ) ) ;
#5035 = ORIENTED_EDGE ( 'NONE', *, *, #17379, .T. ) ;
#5036 = CARTESIAN_POINT ( 'NONE',  ( -7.873497077133136735, 15.44270125396616677, -230.2562282217168672 ) ) ;
#5037 = CARTESIAN_POINT ( 'NONE',  ( -23.67953786836281083, 9.946055673977088674, -229.5560005648173671 ) ) ;
#5038 = CARTESIAN_POINT ( 'NONE',  ( 18.51425713624010427, 11.82474821235740592, -231.3645840199355632 ) ) ;
#5039 = ORIENTED_EDGE ( 'NONE', *, *, #273, .F. ) ;
#5040 = CARTESIAN_POINT ( 'NONE',  ( -4.358491045216396742, -15.83376542237952300, -229.0450454480885583 ) ) ;
#5041 = CARTESIAN_POINT ( 'NONE',  ( 1.387778780781446180E-13, -19.80000000000006111, -78.50000000000000000 ) ) ;
#5042 = ORIENTED_EDGE ( 'NONE', *, *, #13039, .F. ) ;
#5043 = CARTESIAN_POINT ( 'NONE',  ( 25.60482246989237609, 8.614967517510873307, -219.3103232513597618 ) ) ;
#5044 = CARTESIAN_POINT ( 'NONE',  ( 13.35408364068459619, -22.25650632745845314, -229.3239852056058226 ) ) ;
#5045 = CARTESIAN_POINT ( 'NONE',  ( 8.979547488457603421, 23.24376652602565230, -232.6628827740196357 ) ) ;
#5046 = CARTESIAN_POINT ( 'NONE',  ( -28.99926036811508467, 3.909990568804979194, -228.9613767892386988 ) ) ;
#5047 = VECTOR ( 'NONE', #12562, 1000.000000000000000 ) ;
#5048 = CARTESIAN_POINT ( 'NONE',  ( 7.651502705057454889, 16.60422307457919544, -215.4679461133464144 ) ) ;
#5049 = CARTESIAN_POINT ( 'NONE',  ( -14.95675039876920032, 11.42095949000369259, -217.2220932760075129 ) ) ;
#5050 = PRODUCT_DEFINITION ( 'UNKNOWN', '', #20347, #14402 ) ;
#5051 = CARTESIAN_POINT ( 'NONE',  ( -7.189383125363055349, 14.28512618638020548, -231.7475838278701303 ) ) ;
#5052 = CARTESIAN_POINT ( 'NONE',  ( 18.54610009393809023, 0.6523581019769808531, -231.1787333216317677 ) ) ;
#5053 = CARTESIAN_POINT ( 'NONE',  ( 8.510712203779903007, -27.79691582975998898, -230.5316902582456180 ) ) ;
#5054 = CARTESIAN_POINT ( 'NONE',  ( -17.50000000000000711, 0.000000000000000000, -24.99999999999999645 ) ) ;
#5055 = CARTESIAN_POINT ( 'NONE',  ( 0.000000000000000000, 0.000000000000000000, -105.0000000000000000 ) ) ;
#5056 = FACE_OUTER_BOUND ( 'NONE', #16912, .T. ) ;
#5057 = CARTESIAN_POINT ( 'NONE',  ( -26.98548179121306845, 3.096138561569834913, -233.8324893795610251 ) ) ;
#5058 = CARTESIAN_POINT ( 'NONE',  ( -8.537495277687638051, -14.12518193842558212, -230.5589415009361858 ) ) ;
#5059 = DIRECTION ( 'NONE',  ( 1.000000000000000000, 0.000000000000000000, 0.000000000000000000 ) ) ;
#5060 =( LENGTH_UNIT ( ) NAMED_UNIT ( * ) SI_UNIT ( .MILLI., .METRE. ) );
#5061 = CARTESIAN_POINT ( 'NONE',  ( 7.074707374710634156, -26.72731565888815553, -229.5909540767539738 ) ) ;
#5062 = CARTESIAN_POINT ( 'NONE',  ( -20.00523085820573499, 3.356386534894876927, -232.9491364426554298 ) ) ;
#5063 = CARTESIAN_POINT ( 'NONE',  ( 2.485733319737138736, 14.76073968410796056, -221.5245536174130905 ) ) ;
#5064 = CARTESIAN_POINT ( 'NONE',  ( -11.19105919052231179, 21.17456633634251872, -216.2128528132037957 ) ) ;
#5065 = ORIENTED_EDGE ( 'NONE', *, *, #15198, .F. ) ;
#5066 = CARTESIAN_POINT ( 'NONE',  ( -27.87965705189043675, -2.801641921304233840, -225.5825458398584260 ) ) ;
#5067 = ORIENTED_EDGE ( 'NONE', *, *, #21758, .T. ) ;
#5068 = CARTESIAN_POINT ( 'NONE',  ( 18.50911814746675788, 15.92944434255054453, -232.0449215596906072 ) ) ;
#5069 = CARTESIAN_POINT ( 'NONE',  ( -16.66921372850992000, 0.4301828684420727078, -227.8397539831347842 ) ) ;
#5070 = CARTESIAN_POINT ( 'NONE',  ( -18.41237742040652847, 14.06446039901721790, -216.7469276929859632 ) ) ;
#5071 = DIRECTION ( 'NONE',  ( -1.000000000000000000, 0.000000000000000000, 0.000000000000000000 ) ) ;
#5072 = CARTESIAN_POINT ( 'NONE',  ( 17.24952650401854370, 25.19767938110938843, -224.5319471861414797 ) ) ;
#5073 = CARTESIAN_POINT ( 'NONE',  ( -14.47418542577149836, 8.806675964858893479, -228.0010566307936699 ) ) ;
#5074 = CARTESIAN_POINT ( 'NONE',  ( 10.22554538262735413, 24.20440706210576209, -215.6176527921760737 ) ) ;
#5075 = CARTESIAN_POINT ( 'NONE',  ( 22.44730228620155899, 3.608729811217749717, -232.0798239124179645 ) ) ;
#5076 = CARTESIAN_POINT ( 'NONE',  ( -2.916193397327769166, -13.79856165086501107, -222.9033574188488842 ) ) ;
#5077 = ORIENTED_EDGE ( 'NONE', *, *, #1027, .F. ) ;
#5078 = CARTESIAN_POINT ( 'NONE',  ( -9.225692202065292946, -15.38374647092247116, -218.6784895636799320 ) ) ;
#5079 = CARTESIAN_POINT ( 'NONE',  ( -16.13584396029534318, 23.78382729893626646, -231.6788043429177435 ) ) ;
#5080 = CARTESIAN_POINT ( 'NONE',  ( 1.752757082432757185, -17.15725705531007250, -232.7539178101738742 ) ) ;
#5081 = CARTESIAN_POINT ( 'NONE',  ( -6.855867220396999251, 12.17758473459128332, -220.6375607554995213 ) ) ;
#5082 = CARTESIAN_POINT ( 'NONE',  ( 21.68440970896747544, -13.87065835575754846, -215.6285083892243790 ) ) ;
#5083 = CARTESIAN_POINT ( 'NONE',  ( -27.85133024402786006, -1.794102530182491773, -229.4204807338591081 ) ) ;
#5084 = CARTESIAN_POINT ( 'NONE',  ( 13.64836464229338198, 15.83060743948028737, -232.0893758582176929 ) ) ;
#5085 = CARTESIAN_POINT ( 'NONE',  ( -2.993956627714193353, 22.04778837082692178, -231.1741803919495339 ) ) ;
#5086 = CARTESIAN_POINT ( 'NONE',  ( 19.70286159681817750, 17.87637900817293612, -218.6154571368943493 ) ) ;
#5087 = VECTOR ( 'NONE', #1060, 1000.000000000000000 ) ;
#5088 = CARTESIAN_POINT ( 'NONE',  ( 18.23324537670537993, 23.47692953258263771, -224.8333321331434433 ) ) ;
#5089 = CARTESIAN_POINT ( 'NONE',  ( 14.29768887814754663, 10.87030385293788548, -231.8067013864770161 ) ) ;
#5090 = CARTESIAN_POINT ( 'NONE',  ( -0.2114165566986584699, -18.43750818655219703, -233.9360633499430833 ) ) ;
#5091 = CARTESIAN_POINT ( 'NONE',  ( -1.806671251568986669, 13.52068930966770388, -228.3567401718105430 ) ) ;
#5092 = PRODUCT_DEFINITION_SHAPE ( 'NONE', 'NONE',  #22268 ) ;
#5093 = CARTESIAN_POINT ( 'NONE',  ( 27.04607490430786854, 4.607450003618843049, -220.3758934308003461 ) ) ;
#5094 = CARTESIAN_POINT ( 'NONE',  ( 3.085658278449291192, -27.83354332032029888, -231.5475985764057043 ) ) ;
#5095 = CARTESIAN_POINT ( 'NONE',  ( -12.82737030338386219, 8.595865151885988098, -221.6735325378515142 ) ) ;
#5096 = CARTESIAN_POINT ( 'NONE',  ( -1.433739110790628102, 17.19322394474796667, -219.1420620387681879 ) ) ;
#5097 = CARTESIAN_POINT ( 'NONE',  ( -17.42499862437977853, -18.98713029041037004, -232.7811807006768845 ) ) ;
#5098 = CARTESIAN_POINT ( 'NONE',  ( -15.99768154740552717, 2.245235659047613908, -226.7015216759272107 ) ) ;
#5099 = TOROIDAL_SURFACE ( 'NONE', #20909, 12.50000000000000355, 5.000000000000000000 ) ;
#5100 = CARTESIAN_POINT ( 'NONE',  ( 23.04342321161690776, 14.90264581583150694, -218.4777833225197412 ) ) ;
#5101 = EDGE_LOOP ( 'NONE', ( #14716, #20263, #18999, #19285 ) ) ;
#5102 = CARTESIAN_POINT ( 'NONE',  ( 17.68508104102419409, 23.41266195669770767, -227.5327139115408954 ) ) ;
#5103 = CARTESIAN_POINT ( 'NONE',  ( 21.28979032490934031, -14.07620925358629727, -230.4022181401844875 ) ) ;
#5104 = CARTESIAN_POINT ( 'NONE',  ( 24.68599888815047194, -16.20242508705913309, -228.6174911781957633 ) ) ;
#5105 = CARTESIAN_POINT ( 'NONE',  ( 10.02513374692848913, 18.81568788741115128, -217.1505009242214612 ) ) ;
#5106 = CARTESIAN_POINT ( 'NONE',  ( -15.95680269303277221, -1.471987722620473615, -218.5035227479738751 ) ) ;
#5107 = CARTESIAN_POINT ( 'NONE',  ( -8.258403559667634397, -29.80786866836635696, -223.3983869762195127 ) ) ;
#5108 = CARTESIAN_POINT ( 'NONE',  ( 11.39114332821395692, -8.257479203742953189, -226.5648397932267528 ) ) ;
#5109 = CARTESIAN_POINT ( 'NONE',  ( -11.88513743913613752, 17.65694776598872195, -232.6054623148957035 ) ) ;
#5110 = CARTESIAN_POINT ( 'NONE',  ( 11.87550186346493497, 14.27797038184677270, -220.2068243228838185 ) ) ;
#5111 = CARTESIAN_POINT ( 'NONE',  ( -15.15434969228324924, 4.423874646950748613, -230.6144467931089821 ) ) ;
#5112 = CARTESIAN_POINT ( 'NONE',  ( -11.84805200323110164, 5.835720598137266180, -228.2740675967047537 ) ) ;
#5113 = CARTESIAN_POINT ( 'NONE',  ( 13.39541376241636783, -3.462025909069690321, -228.4300562622815391 ) ) ;
#5114 = EDGE_LOOP ( 'NONE', ( #454, #22109, #292, #12348 ) ) ;
#5115 = AXIS2_PLACEMENT_3D ( 'NONE', #20354, #18468, #3144 ) ;
#5116 = CARTESIAN_POINT ( 'NONE',  ( -4.742143146070755932, 15.01230778631049567, -221.4832709320255049 ) ) ;
#5117 = CARTESIAN_POINT ( 'NONE',  ( 11.09231067055629616, 7.417581979752235100, -227.5152062457793534 ) ) ;
#5118 = CARTESIAN_POINT ( 'NONE',  ( 25.12984891811676036, 19.96069634721137476, -226.7154725927711070 ) ) ;
#5119 = CARTESIAN_POINT ( 'NONE',  ( 10.08089751255479527, -9.763210684072014089, -226.4220581413412390 ) ) ;
#5120 = FACE_OUTER_BOUND ( 'NONE', #18374, .T. ) ;
#5121 = ORIENTED_EDGE ( 'NONE', *, *, #10780, .F. ) ;
#5122 = ADVANCED_FACE ( 'NONE', ( #14506 ), #21561, .F. ) ;
#5123 = CARTESIAN_POINT ( 'NONE',  ( -3.060450601941519189, 13.29454208326677289, -222.0135664617158682 ) ) ;
#5124 = CARTESIAN_POINT ( 'NONE',  ( -30.74480097515601074, -10.13586512673612106, -225.7096819839593707 ) ) ;
#5125 = DIRECTION ( 'NONE',  ( 0.000000000000000000, 0.000000000000000000, -1.000000000000000000 ) ) ;
#5126 = CARTESIAN_POINT ( 'NONE',  ( 22.02796522526679723, 16.41909032291435366, -220.1590600991317217 ) ) ;
#5127 = CARTESIAN_POINT ( 'NONE',  ( -16.74550766701807447, 3.787526820511904813, -217.9802846976114381 ) ) ;
#5128 = CARTESIAN_POINT ( 'NONE',  ( 11.32394539683753720, -15.63383003174572572, -233.0723040138117881 ) ) ;
#5129 = CARTESIAN_POINT ( 'NONE',  ( -12.44873260470819787, 7.411970124596155785, -229.4214091473984070 ) ) ;
#5130 = CARTESIAN_POINT ( 'NONE',  ( -15.15110768032078070, 3.517015312212880218, -219.5479300368539270 ) ) ;
#5131 = CARTESIAN_POINT ( 'NONE',  ( -1.434166139689934338, -16.90223958437590213, -219.9603817157532433 ) ) ;
#5132 = CIRCLE ( 'NONE', #10175, 25.00000000000000000 ) ;
#5133 = DIRECTION ( 'NONE',  ( 0.000000000000000000, 0.000000000000000000, 1.000000000000000000 ) ) ;
#5134 = EDGE_CURVE ( 'NONE', #2027, #5173, #4393, .T. ) ;
#5135 = LINE ( 'NONE', #20547, #872 ) ;
#5136 = DIRECTION ( 'NONE',  ( -1.000000000000000000, 0.000000000000000000, 0.000000000000000000 ) ) ;
#5137 = CARTESIAN_POINT ( 'NONE',  ( 23.84477361619719105, -14.51625201957343592, -224.2863126538025540 ) ) ;
#5138 = CARTESIAN_POINT ( 'NONE',  ( 12.80332909036350308, -2.946706566599696320, -225.5941091591410839 ) ) ;
#5139 = CARTESIAN_POINT ( 'NONE',  ( -20.75182054862913006, -9.917826596856404109, 1.322042766941443626 ) ) ;
#5140 = CARTESIAN_POINT ( 'NONE',  ( 18.90025403853754327, 17.70150481658638952, -229.5234643039372315 ) ) ;
#5141 = CARTESIAN_POINT ( 'NONE',  ( 0.9879969248128627202, 20.02408072508558945, -218.2055348255049410 ) ) ;
#5142 = EDGE_CURVE ( 'NONE', #8407, #11804, #15175, .T. ) ;
#5143 = CARTESIAN_POINT ( 'NONE',  ( 7.462112298232926655, -14.04285870004232528, -232.2430251799377174 ) ) ;
#5144 = CARTESIAN_POINT ( 'NONE',  ( 17.15627899979664051, -18.64955541608202694, -217.1729447097152388 ) ) ;
#5145 = ORIENTED_EDGE ( 'NONE', *, *, #22146, .T. ) ;
#5146 = CARTESIAN_POINT ( 'NONE',  ( -9.661739055621840322, 20.41227307912577871, -232.0920144483423257 ) ) ;
#5147 = CARTESIAN_POINT ( 'NONE',  ( -25.36936018126600345, 11.57160208538938306, -224.9662154788713622 ) ) ;
#5148 = CARTESIAN_POINT ( 'NONE',  ( 14.23294950300690331, 6.961167337017927892, -222.0879133937260974 ) ) ;
#5149 = CARTESIAN_POINT ( 'NONE',  ( -8.698852260299409167, -27.05211559305675451, -224.0453856107860986 ) ) ;
#5150 = LINE ( 'NONE', #8213, #16618 ) ;
#5151 = VECTOR ( 'NONE', #18428, 1000.000000000000000 ) ;
#5152 = ORIENTED_EDGE ( 'NONE', *, *, #22017, .T. ) ;
#5153 = CIRCLE ( 'NONE', #20226, 21.00000000000008527 ) ;
#5154 = CARTESIAN_POINT ( 'NONE',  ( 20.02669998934234741, 11.93441252203826508, -216.7824909737982182 ) ) ;
#5155 = CARTESIAN_POINT ( 'NONE',  ( 10.74448773353722686, -20.82765299830942851, -219.2305132457354659 ) ) ;
#5156 = CARTESIAN_POINT ( 'NONE',  ( 4.343013938751969505, 13.02036404005131587, -224.7825435359082178 ) ) ;
#5157 = CARTESIAN_POINT ( 'NONE',  ( -6.571166997218196748, 12.74865329367398736, -229.9840124400968762 ) ) ;
#5158 = CARTESIAN_POINT ( 'NONE',  ( 13.72784977962315267, 2.687686193488206143, -220.8507880271885995 ) ) ;
#5159 = CARTESIAN_POINT ( 'NONE',  ( -2.772442535524381579, 13.75675912271027457, -228.9770533867650215 ) ) ;
#5160 = CARTESIAN_POINT ( 'NONE',  ( 10.37371678005726139, 3.577098705721246219, 91.99999999999998579 ) ) ;
#5161 = CIRCLE ( 'NONE', #4088, 17.95451841861686049 ) ;
#5162 = CARTESIAN_POINT ( 'NONE',  ( 1.836136847161299990, -12.84546502099244591, -226.1727064218434293 ) ) ;
#5163 = CARTESIAN_POINT ( 'NONE',  ( 16.06750045776299629, -1.909440863493336860, -220.4398626676318713 ) ) ;
#5164 = LINE ( 'NONE', #8338, #3403 ) ;
#5165 = AXIS2_PLACEMENT_3D ( 'NONE', #19638, #17970, #9201 ) ;
#5166 = CARTESIAN_POINT ( 'NONE',  ( -17.21167111787709914, -1.850592482912338799, -230.8442569545952665 ) ) ;
#5167 = CARTESIAN_POINT ( 'NONE',  ( -27.68973657932738064, 5.930811633061950694, -216.7842770206311513 ) ) ;
#5168 = CARTESIAN_POINT ( 'NONE',  ( -15.71547198132422984, -24.70787285779005060, -226.7356521228395536 ) ) ;
#5169 = CARTESIAN_POINT ( 'NONE',  ( 12.78854151797817451, -25.92021405714643123, -222.0152117995072842 ) ) ;
#5170 = CARTESIAN_POINT ( 'NONE',  ( 16.48801037644500056, 3.165716804515234628, -216.8169430726136113 ) ) ;
#5171 = CARTESIAN_POINT ( 'NONE',  ( 5.359747511823000465, 20.14556701535824601, -232.9094821222151381 ) ) ;
#5172 = CARTESIAN_POINT ( 'NONE',  ( -23.16143087541734502, 21.36835206473086046, -221.8715256527013651 ) ) ;
#5173 = VERTEX_POINT ( 'NONE', #3441 ) ;
#5174 = CARTESIAN_POINT ( 'NONE',  ( 11.86238739854314872, -1.469869507039519130, -223.6725020993723660 ) ) ;
#5175 = VERTEX_POINT ( 'NONE', #22008 ) ;
#5176 = CARTESIAN_POINT ( 'NONE',  ( 11.33210854356620523, 22.81476816607802149, -217.8536224460118262 ) ) ;
#5177 = CARTESIAN_POINT ( 'NONE',  ( -19.92987771446595957, 11.92619342620000999, -232.5382020162021206 ) ) ;
#5178 = CARTESIAN_POINT ( 'NONE',  ( -24.30769394037691100, 17.48612956801762053, -223.4340414801748693 ) ) ;
#5179 = CARTESIAN_POINT ( 'NONE',  ( -10.95598939193837928, -18.74794674280272488, -217.4432683290776538 ) ) ;
#5180 = CARTESIAN_POINT ( 'NONE',  ( -12.50000000000000355, 1.530808498934191916E-15, -65.00000000000000000 ) ) ;
#5181 = DIRECTION ( 'NONE',  ( 1.000000000000000000, 0.000000000000000000, 0.000000000000000000 ) ) ;
#5182 = AXIS2_PLACEMENT_3D ( 'NONE', #1960, #5556, #20632 ) ;
#5183 = CARTESIAN_POINT ( 'NONE',  ( -24.48812334466693486, 4.469247780253509106, -230.3044243311433945 ) ) ;
#5184 = CARTESIAN_POINT ( 'NONE',  ( 18.15173157547545557, 23.32481284044927961, -217.8532150843729482 ) ) ;
#5185 = ADVANCED_FACE ( 'NONE', ( #10321 ), #6944, .F. ) ;
#5186 = CARTESIAN_POINT ( 'NONE',  ( 22.90621760533471019, 17.25363305745006670, -230.8615280072714597 ) ) ;
#5187 = CARTESIAN_POINT ( 'NONE',  ( -13.06588638656279322, -26.69120070130052014, -220.2265807429280642 ) ) ;
#5188 = ORIENTED_EDGE ( 'NONE', *, *, #15930, .T. ) ;
#5189 = CARTESIAN_POINT ( 'NONE',  ( -5.688232406366994454, -14.80527619068227629, -228.6723097085491645 ) ) ;
#5190 = CARTESIAN_POINT ( 'NONE',  ( -7.099035520468861549, 19.73710792467281649, -233.8745459908100770 ) ) ;
#5191 = CARTESIAN_POINT ( 'NONE',  ( 12.73130673999417795, -23.76414828096303467, -217.7386337832039942 ) ) ;
#5192 = CARTESIAN_POINT ( 'NONE',  ( -2.772442535524381579, 13.75675912271027457, -228.9770533867650215 ) ) ;
#5193 = CARTESIAN_POINT ( 'NONE',  ( 10.88154471369483112, -8.002597937117323923, -230.2267818776996080 ) ) ;
#5194 = CARTESIAN_POINT ( 'NONE',  ( -21.08965452150356867, -10.66825825602615296, -217.1903588586143314 ) ) ;
#5195 = CARTESIAN_POINT ( 'NONE',  ( 15.89621445970763070, 6.639162626453350313, -232.5295318698041456 ) ) ;
#5196 = CARTESIAN_POINT ( 'NONE',  ( -2.906906946766868227, 27.66682465340607422, -226.6559963821499082 ) ) ;
#5197 = CARTESIAN_POINT ( 'NONE',  ( -18.88895772509644644, 1.306698388790553444, -217.6272550812279292 ) ) ;
#5198 = CIRCLE ( 'NONE', #540, 17.50000000000000355 ) ;
#5199 = CARTESIAN_POINT ( 'NONE',  ( 13.49011766416699842, 7.659170998773840111, -228.1905628957712793 ) ) ;
#5200 = CARTESIAN_POINT ( 'NONE',  ( 17.41909632439413969, 2.006477695503792624, -233.4081875040758121 ) ) ;
#5201 = CARTESIAN_POINT ( 'NONE',  ( 4.449544252370068342, -12.87211356511098082, -219.5022864574935113 ) ) ;
#5202 = CARTESIAN_POINT ( 'NONE',  ( 18.65058977333779211, 24.40868228550881014, -219.3406275662563303 ) ) ;
#5203 = DIRECTION ( 'NONE',  ( 0.000000000000000000, 0.000000000000000000, -1.000000000000000000 ) ) ;
#5204 = CARTESIAN_POINT ( 'NONE',  ( 13.43185000535467211, -22.27464880184020757, -218.9084381759842870 ) ) ;
#5205 = CARTESIAN_POINT ( 'NONE',  ( -12.78923236353123727, 15.53885160143439315, -231.8946633672937878 ) ) ;
#5206 = CARTESIAN_POINT ( 'NONE',  ( -4.691002462566371101, 21.98518063340150164, -232.2516024630330094 ) ) ;
#5207 = EDGE_CURVE ( 'NONE', #10297, #15308, #1761, .T. ) ;
#5208 = CARTESIAN_POINT ( 'NONE',  ( -18.75993824683981970, -9.028840681436806292, -217.1556094966459227 ) ) ;
#5209 = CARTESIAN_POINT ( 'NONE',  ( -15.65611835717891687, 5.486779671999271635, -227.0554626315911264 ) ) ;
#5211 = CARTESIAN_POINT ( 'NONE',  ( 18.39533937270110187, 14.26564464607222504, -233.9088367426310242 ) ) ;
#5210 = AXIS2_PLACEMENT_3D ( 'NONE', #14631, #14520, #21354 ) ;
#5212 = EDGE_LOOP ( 'NONE', ( #21846, #11544, #14180, #4549 ) ) ;
#5213 = CARTESIAN_POINT ( 'NONE',  ( 8.329997790135040603, 12.51216704542961899, -228.7022893680961602 ) ) ;
#5214 = CARTESIAN_POINT ( 'NONE',  ( 24.55456120837795808, -10.86188008310946351, -220.0712554825904590 ) ) ;
#5215 = VECTOR ( 'NONE', #13771, 1000.000000000000000 ) ;
#5216 = ORIENTED_EDGE ( 'NONE', *, *, #21646, .F. ) ;
#5217 = CARTESIAN_POINT ( 'NONE',  ( 12.94117841657163126, -3.283311917827119064, -226.8844617769393039 ) ) ;
#5218 = DIRECTION ( 'NONE',  ( 0.000000000000000000, 1.000000000000000000, 0.000000000000000000 ) ) ;
#5219 = CARTESIAN_POINT ( 'NONE',  ( 22.86997486125673618, 17.56009411325475966, -222.3578648042903296 ) ) ;
#5220 = CARTESIAN_POINT ( 'NONE',  ( -15.30224200789663946, -6.308083384910589508, -216.9633489813582514 ) ) ;
#5221 = CARTESIAN_POINT ( 'NONE',  ( -1.890995374385051608, -13.09686096954197509, -227.5694739903412085 ) ) ;
#5222 = CARTESIAN_POINT ( 'NONE',  ( 9.918856707546316542, -11.48950767347732871, -219.9734948840342668 ) ) ;
#5223 = CARTESIAN_POINT ( 'NONE',  ( 0.4762409465891800919, 16.20008108839776284, -225.9988706007428050 ) ) ;
#5224 = DIRECTION ( 'NONE',  ( 0.000000000000000000, 0.000000000000000000, -1.000000000000000000 ) ) ;
#5225 = CARTESIAN_POINT ( 'NONE',  ( 14.68130101653174613, 6.427210486143660084, -228.0153742661088074 ) ) ;
#5226 = CARTESIAN_POINT ( 'NONE',  ( -13.56774755469388616, 7.311522441667196226, -219.1912666243428021 ) ) ;
#5227 = CARTESIAN_POINT ( 'NONE',  ( -3.389634396460917465, 16.42708991135657115, -221.9057377485790994 ) ) ;
#5228 = CARTESIAN_POINT ( 'NONE',  ( 18.43413881788024611, -3.292634616013774274, -216.7808090690139409 ) ) ;
#5229 = CARTESIAN_POINT ( 'NONE',  ( 2.464084843620814702, 29.35663482419208492, -227.0015060686748143 ) ) ;
#5230 = CARTESIAN_POINT ( 'NONE',  ( -17.55809605150417951, 6.636094600389130349, -229.8856864643722986 ) ) ;
#5231 = CARTESIAN_POINT ( 'NONE',  ( 10.66732316618037402, 25.78610527446713263, -216.5597036843431624 ) ) ;
#5232 = CARTESIAN_POINT ( 'NONE',  ( 5.719431426348611680, -15.09047950350996281, -220.7788505835459318 ) ) ;
#5233 = CARTESIAN_POINT ( 'NONE',  ( 0.000000000000000000, 21.00000000000006395, 75.00000000000000000 ) ) ;
#5234 = ORIENTED_EDGE ( 'NONE', *, *, #19552, .F. ) ;
#5235 = CARTESIAN_POINT ( 'NONE',  ( 1.382955251742491898, 16.46353944795171032, -231.7743150979565030 ) ) ;
#5236 = CARTESIAN_POINT ( 'NONE',  ( -8.465184826868526358, -8.692222964613778302, -225.5402182279159149 ) ) ;
#5237 = LINE ( 'NONE', #13472, #19455 ) ;
#5238 = CARTESIAN_POINT ( 'NONE',  ( 25.18785298611088308, 3.974282393449815931, -218.7636041058819956 ) ) ;
#5239 = CARTESIAN_POINT ( 'NONE',  ( -20.54164754914381064, 7.122791156791981493, -233.5720402887671980 ) ) ;
#5240 = CARTESIAN_POINT ( 'NONE',  ( 17.28140336138120858, -11.48510652344925020, -216.9852223368602893 ) ) ;
#5241 = CARTESIAN_POINT ( 'NONE',  ( -29.88125065636863198, 4.504452993877526623, -226.2048141718237275 ) ) ;
#5242 = CARTESIAN_POINT ( 'NONE',  ( -14.10849459794400751, -0.2436790717799666162, -223.1085195285415921 ) ) ;
#5243 = CARTESIAN_POINT ( 'NONE',  ( -8.652743106909156268, -19.89692808811530966, -232.3032230114403376 ) ) ;
#5244 = CARTESIAN_POINT ( 'NONE',  ( 0.000000000000000000, 0.000000000000000000, -30.00000000000000000 ) ) ;
#5245 = CARTESIAN_POINT ( 'NONE',  ( -21.18273580851505145, 8.962137229497693980, 4.448298016007305122 ) ) ;
#5246 = CARTESIAN_POINT ( 'NONE',  ( -23.49379658590067876, 11.46840048879614393, -217.2519070826072323 ) ) ;
#5247 = CARTESIAN_POINT ( 'NONE',  ( 19.11859169356911536, -17.02155004481861411, -230.1485466288596911 ) ) ;
#5248 = CIRCLE ( 'NONE', #17491, 2.100000000000000089 ) ;
#5250 = EDGE_CURVE ( 'NONE', #21337, #12667, #10141, .T. ) ;
#5249 = DIRECTION ( 'NONE',  ( -1.000000000000000000, 0.000000000000000000, 0.000000000000000000 ) ) ;
#5251 = DIRECTION ( 'NONE',  ( 1.000000000000000000, -0.000000000000000000, -0.000000000000000000 ) ) ;
#5252 = CARTESIAN_POINT ( 'NONE',  ( 15.99247752609008444, 10.72268246046808216, -230.5614800526110173 ) ) ;
#5253 = CARTESIAN_POINT ( 'NONE',  ( -12.22073052649759184, 14.03927388329973525, -215.9097966823721606 ) ) ;
#5254 = CARTESIAN_POINT ( 'NONE',  ( 10.90137817157632227, 16.64712710991609868, -230.5401786220292593 ) ) ;
#5255 = CARTESIAN_POINT ( 'NONE',  ( -1.044869047506413517, -25.54243019362050404, -231.6194713969048564 ) ) ;
#5256 = CARTESIAN_POINT ( 'NONE',  ( 21.04926289057418742, -6.455467962217539934, -215.4677037730695872 ) ) ;
#5257 = ORIENTED_EDGE ( 'NONE', *, *, #13812, .T. ) ;
#5258 = CARTESIAN_POINT ( 'NONE',  ( -12.87285471141929172, 9.485162256560764504, -229.1865421006261840 ) ) ;
#5259 = CARTESIAN_POINT ( 'NONE',  ( -16.51501534778698854, 10.61825396983174485, -230.5082364903317966 ) ) ;
#5260 = CARTESIAN_POINT ( 'NONE',  ( -31.04267853410473421, 7.029517189377418873, -226.8060334161593516 ) ) ;
#5261 = CARTESIAN_POINT ( 'NONE',  ( -1.494569538902034145, -28.29191435206508487, -228.8702894339512852 ) ) ;
#5262 = DIRECTION ( 'NONE',  ( 1.000000000000000000, 0.000000000000000000, 0.000000000000000000 ) ) ;
#5263 = ORIENTED_EDGE ( 'NONE', *, *, #6961, .F. ) ;
#5264 = CARTESIAN_POINT ( 'NONE',  ( 22.90621760533471019, 17.25363305745006670, -230.8615280072714597 ) ) ;
#5265 = CARTESIAN_POINT ( 'NONE',  ( 7.764422566766373990, -15.81008911711046672, -220.9836405809557220 ) ) ;
#5266 = CARTESIAN_POINT ( 'NONE',  ( 18.23324537670537993, 23.47692953258263771, -224.8333321331434433 ) ) ;
#5267 = CARTESIAN_POINT ( 'NONE',  ( -6.201839134465864767, 11.37481922992157379, -223.7040893475979146 ) ) ;
#5268 = CARTESIAN_POINT ( 'NONE',  ( 24.19672885113291727, 10.99915907690374439, -233.6834417629405891 ) ) ;
#5269 = CARTESIAN_POINT ( 'NONE',  ( 5.331555957413248059, 27.50712867803999728, -219.0801070358024276 ) ) ;
#5270 = CARTESIAN_POINT ( 'NONE',  ( 13.43288712491620629, 0.9237972417345811094, -222.1423753579431946 ) ) ;
#5271 = CARTESIAN_POINT ( 'NONE',  ( -6.642805165258356404, -28.12267032419628521, -230.9452027245340560 ) ) ;
#5272 = CARTESIAN_POINT ( 'NONE',  ( 11.78320976064766690, -8.193118641535518165, -222.2581747538435479 ) ) ;
#5273 = FACE_OUTER_BOUND ( 'NONE', #16255, .T. ) ;
#5274 = DIRECTION ( 'NONE',  ( 0.000000000000000000, 0.000000000000000000, 1.000000000000000000 ) ) ;
#5275 = CARTESIAN_POINT ( 'NONE',  ( 28.02123297569005089, 5.903198806000402143, -227.5759114383273811 ) ) ;
#5276 = CARTESIAN_POINT ( 'NONE',  ( -15.79547310275335725, -3.553268508742920773, -224.0225025563328813 ) ) ;
#5277 = SHAPE_REPRESENTATION ( 'BR-822', ( #11745, #1257, #13854, #15648, #19270, #7080, #14269, #9948, #13909 ), #16774 ) ;
#5278 = CARTESIAN_POINT ( 'NONE',  ( 17.23039831256031817, 3.331158952577910615, -216.4027685342793461 ) ) ;
#5279 = CARTESIAN_POINT ( 'NONE',  ( 0.1556102272723409452, 19.71550568250159685, -232.1993058477363547 ) ) ;
#5280 = CARTESIAN_POINT ( 'NONE',  ( 2.208705534715813101, 15.26926593729510984, -227.3643075380122980 ) ) ;
#5281 = ORIENTED_EDGE ( 'NONE', *, *, #11865, .T. ) ;
#5282 = CARTESIAN_POINT ( 'NONE',  ( -25.18517655442826353, -3.313270981248286340, -229.9274946033256697 ) ) ;
#5283 = EDGE_LOOP ( 'NONE', ( #18489, #9456, #17732, #12070, #11506, #9170 ) ) ;
#5284 = CARTESIAN_POINT ( 'NONE',  ( 17.97843143658897347, 22.12221935793617078, -220.9346589834416079 ) ) ;
#5285 = CARTESIAN_POINT ( 'NONE',  ( -16.09559989144903369, 12.31939076846282966, -216.7948290530243298 ) ) ;
#5286 = CARTESIAN_POINT ( 'NONE',  ( -14.58670098223046629, 7.239570004716886942, -229.3284954533748135 ) ) ;
#5287 = CARTESIAN_POINT ( 'NONE',  ( -15.28220591200235390, -15.65475725988279443, -217.1155325995422913 ) ) ;
#5288 = EDGE_CURVE ( 'NONE', #1564, #1604, #6892, .T. ) ;
#5289 = CARTESIAN_POINT ( 'NONE',  ( -14.70651859537745487, 4.211702956367679107, -230.0357207626005334 ) ) ;
#5290 = CARTESIAN_POINT ( 'NONE',  ( -22.00000000000137490, -2.602085213965210642E-15, -216.9999999999999716 ) ) ;
#5291 = FACE_OUTER_BOUND ( 'NONE', #17619, .T. ) ;
#5292 = CARTESIAN_POINT ( 'NONE',  ( 21.72366288329714834, 2.385777479048636351, -215.9150265590827757 ) ) ;
#5293 = CARTESIAN_POINT ( 'NONE',  ( -9.007976471255481954, 12.60968992764439633, -227.9367755778692981 ) ) ;
#5294 = CARTESIAN_POINT ( 'NONE',  ( 8.865150807857233417, 8.939496441981303221, -220.7647208555746090 ) ) ;
#5295 = CARTESIAN_POINT ( 'NONE',  ( 21.19180206786061405, -1.472355559550188264, -231.3901500139509722 ) ) ;
#5296 = CARTESIAN_POINT ( 'NONE',  ( -29.95626564321166541, -9.027512590954497540, -220.3228832733970819 ) ) ;
#5297 = CARTESIAN_POINT ( 'NONE',  ( -24.95227886253013239, -16.82584358170602101, -223.8363818545792299 ) ) ;
#5298 = CARTESIAN_POINT ( 'NONE',  ( -16.58369694688956741, 24.75758513462668375, -230.3405478298966784 ) ) ;
#5299 = CARTESIAN_POINT ( 'NONE',  ( -1.778254167844783851, -12.78790610364390012, -225.9413532495922254 ) ) ;
#5300 = CARTESIAN_POINT ( 'NONE',  ( -6.101488798441174310, 11.33371047077072369, -225.3616985956418546 ) ) ;
#5301 = CARTESIAN_POINT ( 'NONE',  ( 12.37876697492742650, -4.127359938151530905, -227.8507160500782618 ) ) ;
#5302 = CARTESIAN_POINT ( 'NONE',  ( -28.87859926594958537, -0.8320174534291842061, -222.6356913548140142 ) ) ;
#5303 = CARTESIAN_POINT ( 'NONE',  ( -21.28183200535960040, 1.085030287403131233, -217.0000000015322712 ) ) ;
#5304 = DIRECTION ( 'NONE',  ( -1.000000000000000000, 0.000000000000000000, 0.000000000000000000 ) ) ;
#5305 = CARTESIAN_POINT ( 'NONE',  ( -3.125843203957122896, 15.99774916147792680, -222.8808123721668721 ) ) ;
#5306 = CARTESIAN_POINT ( 'NONE',  ( 26.75666476377482539, 8.100664119735744961, -232.1611550320539834 ) ) ;
#5307 = CARTESIAN_POINT ( 'NONE',  ( 18.46552355142154411, 5.019711608606525211, -231.5099115070375433 ) ) ;
#5308 = CARTESIAN_POINT ( 'NONE',  ( 13.71882454279727526, 6.278400000045776252, -230.2269611870541723 ) ) ;
#5309 = CARTESIAN_POINT ( 'NONE',  ( 6.571750410407496190, -24.62545695199335682, -234.5391748598602248 ) ) ;
#5310 = CARTESIAN_POINT ( 'NONE',  ( 5.030854775705693172, 19.94152319263364603, -234.9034581965229336 ) ) ;
#5311 = CARTESIAN_POINT ( 'NONE',  ( 17.34727976380017722, 4.822939981779328811, -230.8836217450937909 ) ) ;
#5312 = CARTESIAN_POINT ( 'NONE',  ( -14.63769981573866552, -28.59145599960802642, -226.8825043222271631 ) ) ;
#5313 = CARTESIAN_POINT ( 'NONE',  ( -8.435479365662203577, 14.12888021429238528, -220.5365774424437859 ) ) ;
#5314 = CARTESIAN_POINT ( 'NONE',  ( 11.01659168199870287, 19.17922986229587323, -233.3715978632214387 ) ) ;
#5315 = CARTESIAN_POINT ( 'NONE',  ( -23.10791503177032880, -5.282985115830100220, -217.6364121950018671 ) ) ;
#5316 = CARTESIAN_POINT ( 'NONE',  ( -16.51501534778698854, 10.61825396983174485, -230.5082364903317966 ) ) ;
#5317 = AXIS2_PLACEMENT_3D ( 'NONE', #11889, #6371, #14944 ) ;
#5318 = CARTESIAN_POINT ( 'NONE',  ( -23.89856910807799295, 17.42297078648622843, -222.0178620725767757 ) ) ;
#5319 = CARTESIAN_POINT ( 'NONE',  ( 18.84307465506600465, 4.899879697440840509, -218.2189947030338715 ) ) ;
#5320 = EDGE_LOOP ( 'NONE', ( #21785, #9674, #18201, #2573 ) ) ;
#5321 = CARTESIAN_POINT ( 'NONE',  ( 4.484811161826725900, 15.38298568785217313, -219.4617573400562662 ) ) ;
#5322 = CARTESIAN_POINT ( 'NONE',  ( 13.59384321027942910, -22.95766697980085169, -228.5239052398278830 ) ) ;
#5323 = ORIENTED_EDGE ( 'NONE', *, *, #3630, .F. ) ;
#5324 = CARTESIAN_POINT ( 'NONE',  ( 14.41459438711767760, -7.262430563887544821, -219.0449948566021021 ) ) ;
#5325 = CARTESIAN_POINT ( 'NONE',  ( -9.106229537879125147, 25.89784491087598184, -228.9807674929363372 ) ) ;
#5326 = EDGE_CURVE ( 'NONE', #2937, #11287, #4367, .T. ) ;
#5327 = CARTESIAN_POINT ( 'NONE',  ( 9.107417252317809186, 16.30291009569977234, -218.0131178633739921 ) ) ;
#5328 = CARTESIAN_POINT ( 'NONE',  ( -10.70714119831929168, -8.316548062297686172, -219.3892619542279192 ) ) ;
#5329 = CARTESIAN_POINT ( 'NONE',  ( -3.300598509645395584, -18.18730530649546395, -233.4303386612170925 ) ) ;
#5330 = CARTESIAN_POINT ( 'NONE',  ( -1.643553855084622928, -13.05119293000219294, -222.7191902239112551 ) ) ;
#5331 = CARTESIAN_POINT ( 'NONE',  ( 0.04449911090679885967, 16.51968908208873899, -222.9067194156212111 ) ) ;
#5332 = DIRECTION ( 'NONE',  ( 0.000000000000000000, 0.000000000000000000, 1.000000000000000000 ) ) ;
#5333 = CARTESIAN_POINT ( 'NONE',  ( 22.37742875470728876, 11.29804624588327577, -218.9256858961603882 ) ) ;
#5334 = CARTESIAN_POINT ( 'NONE',  ( -28.59157645096996347, 5.137867505054540374, -220.4667042235044505 ) ) ;
#5335 = CARTESIAN_POINT ( 'NONE',  ( -7.928079932584687128, 26.12067226064367986, -221.2051195461628197 ) ) ;
#5336 = CARTESIAN_POINT ( 'NONE',  ( 9.336393807558161839, 27.79372469574263960, -228.5913636680961361 ) ) ;
#5337 = CARTESIAN_POINT ( 'NONE',  ( -26.64664107080812627, 5.256684826493772000, -228.0533579629717735 ) ) ;
#5338 = CARTESIAN_POINT ( 'NONE',  ( 16.84354851290083133, 10.42424693870724361, -215.2582953371023109 ) ) ;
#5339 = CIRCLE ( 'NONE', #13989, 5.000000000000000888 ) ;
#5340 = CARTESIAN_POINT ( 'NONE',  ( 15.50624253654579654, -15.96056326703506478, -233.0338314371582840 ) ) ;
#5341 = LINE ( 'NONE', #12223, #10018 ) ;
#5342 = ORIENTED_EDGE ( 'NONE', *, *, #4652, .T. ) ;
#5343 = CARTESIAN_POINT ( 'NONE',  ( -2.817219543927646175, 14.13981714106644993, -229.6779615865167443 ) ) ;
#5344 = CARTESIAN_POINT ( 'NONE',  ( -23.67094103897667523, 1.103242709927489740, -215.1660654633311935 ) ) ;
#5345 = CARTESIAN_POINT ( 'NONE',  ( 22.36788034568564854, -2.140002702436959225, -217.7104380410378610 ) ) ;
#5346 = CARTESIAN_POINT ( 'NONE',  ( 12.85408565574548412, 7.821283853063205171, -223.1248833997948111 ) ) ;
#5347 = CARTESIAN_POINT ( 'NONE',  ( -16.71711190488355570, 0.6105529133557690002, -230.9511258789794681 ) ) ;
#5348 = CARTESIAN_POINT ( 'NONE',  ( 15.65513449100897780, -26.00057195821942457, -227.4103383097017570 ) ) ;
#5349 = CARTESIAN_POINT ( 'NONE',  ( -14.83974801774860630, 13.71714848582103485, -216.0935642439352762 ) ) ;
#5350 = ORIENTED_EDGE ( 'NONE', *, *, #5326, .F. ) ;
#5351 = CARTESIAN_POINT ( 'NONE',  ( -25.80904414196669450, 12.19501778665756220, -219.1732313092283846 ) ) ;
#5352 = CARTESIAN_POINT ( 'NONE',  ( -16.87231408860552051, -20.68405295654727993, -231.0270656955280515 ) ) ;
#5353 = CARTESIAN_POINT ( 'NONE',  ( 1.665334536937735316E-13, -24.63401512838760610, 77.51594804401857175 ) ) ;
#5354 = CARTESIAN_POINT ( 'NONE',  ( 0.000000000000000000, 0.000000000000000000, 77.51594804401857175 ) ) ;
#5355 = CARTESIAN_POINT ( 'NONE',  ( -20.54164754914381064, 7.122791156791981493, -233.5720402887671980 ) ) ;
#5356 = CARTESIAN_POINT ( 'NONE',  ( 15.78601976571614962, -10.64697985159532401, -219.7411765650222151 ) ) ;
#5357 = CARTESIAN_POINT ( 'NONE',  ( -28.55814054826834791, -1.660722980825670048, -228.2640858091212408 ) ) ;
#5358 = CARTESIAN_POINT ( 'NONE',  ( 25.50000000000000000, -3.600000000000001421, -2.699999999999999289 ) ) ;
#5359 = CARTESIAN_POINT ( 'NONE',  ( 14.04819512851487673, 6.831178966487911453, -222.6676118107292552 ) ) ;
#5360 = CARTESIAN_POINT ( 'NONE',  ( -8.201407585998298444, 17.38801480109368924, -216.6295241303755006 ) ) ;
#5361 = CARTESIAN_POINT ( 'NONE',  ( 25.18311526135610734, 13.65721788432563955, -224.7326014392022273 ) ) ;
#5362 = CARTESIAN_POINT ( 'NONE',  ( -0.004649462380863607185, -15.32103018016390017, -221.8331694311728484 ) ) ;
#5363 = CARTESIAN_POINT ( 'NONE',  ( 13.04627209130898002, -4.074791396861574988, -220.3858784301183675 ) ) ;
#5364 = EDGE_LOOP ( 'NONE', ( #11204, #4448, #4126, #60 ) ) ;
#5365 = CARTESIAN_POINT ( 'NONE',  ( -4.130417896617784912, 16.21758012034559826, -229.8171973319304584 ) ) ;
#5366 = CARTESIAN_POINT ( 'NONE',  ( -26.35007260221545877, 6.140745174321167177, -221.9336216792591188 ) ) ;
#5367 = CARTESIAN_POINT ( 'NONE',  ( 20.62963957373278134, 2.372686805184054837, -232.5966151263358483 ) ) ;
#5368 = CARTESIAN_POINT ( 'NONE',  ( -22.93762879021373280, -16.04239672171475206, -226.2337446402420653 ) ) ;
#5369 = DIRECTION ( 'NONE',  ( 0.000000000000000000, 0.000000000000000000, 1.000000000000000000 ) ) ;
#5370 = ORIENTED_EDGE ( 'NONE', *, *, #6806, .T. ) ;
#5371 = CARTESIAN_POINT ( 'NONE',  ( 28.62253243811995418, 3.652502539191337494, -225.4068779441649326 ) ) ;
#5372 = CARTESIAN_POINT ( 'NONE',  ( 3.608972370552595343, -15.05750810295313435, -224.7555151483228713 ) ) ;
#5373 = CARTESIAN_POINT ( 'NONE',  ( 13.61707622192329481, 14.84143455326118932, -217.6958999636067063 ) ) ;
#5374 = CARTESIAN_POINT ( 'NONE',  ( -11.69688825528096388, 18.63404371591177622, -215.8612738028812714 ) ) ;
#5375 = EDGE_CURVE ( 'NONE', #18785, #9979, #5237, .T. ) ;
#5376 = CARTESIAN_POINT ( 'NONE',  ( 15.65443801613259467, 7.488839228060037989, -233.6469817377710569 ) ) ;
#5377 = CARTESIAN_POINT ( 'NONE',  ( 7.769483725421269860, 20.68783433326350263, -233.2348178266662728 ) ) ;
#5378 = CARTESIAN_POINT ( 'NONE',  ( 14.01840907662334956, 2.035826308177659083, -222.7954063512536038 ) ) ;
#5379 = CARTESIAN_POINT ( 'NONE',  ( 1.799766247726228174, -14.75051420185460849, -230.6199496058247291 ) ) ;
#5380 = CARTESIAN_POINT ( 'NONE',  ( 8.785770181087007913, -10.38731345016515917, -223.4272116603623317 ) ) ;
#5381 = DIRECTION ( 'NONE',  ( -1.000000000000000000, 0.000000000000000000, 0.000000000000000000 ) ) ;
#5382 = CARTESIAN_POINT ( 'NONE',  ( -9.045741320599788082, 11.46901338045063312, -219.0588111342715365 ) ) ;
#5383 = CARTESIAN_POINT ( 'NONE',  ( -24.91054099106560926, -7.366054470814448862, -220.6971974931307159 ) ) ;
#5384 = CARTESIAN_POINT ( 'NONE',  ( 14.55590852435181226, 2.816890518231522034, -218.5131513550309990 ) ) ;
#5385 = CARTESIAN_POINT ( 'NONE',  ( 7.450672702945051462, 17.42371045663376705, -217.2894981592719432 ) ) ;
#5386 = CARTESIAN_POINT ( 'NONE',  ( -1.470815287892122125, 29.54293232078718745, -224.5855911371830302 ) ) ;
#5387 = ORIENTED_EDGE ( 'NONE', *, *, #10065, .T. ) ;
#5388 = CARTESIAN_POINT ( 'NONE',  ( 15.19497947618244460, -8.176986896541109218, -234.2449823452919304 ) ) ;
#5389 = EDGE_LOOP ( 'NONE', ( #8142, #17844, #20869, #7146, #830, #18701 ) ) ;
#5390 = CARTESIAN_POINT ( 'NONE',  ( 19.72515656911863147, 14.02277373989196541, -218.0718040828188009 ) ) ;
#5391 = CARTESIAN_POINT ( 'NONE',  ( -8.929606928624414408, 11.65278034267609186, -219.1999234847403386 ) ) ;
#5392 = CARTESIAN_POINT ( 'NONE',  ( -15.10945752141584464, 6.470132813599071220, -220.1568141593501764 ) ) ;
#5393 = CARTESIAN_POINT ( 'NONE',  ( -5.688232406366994454, -14.80527619068227629, -228.6723097085491645 ) ) ;
#5394 = DIRECTION ( 'NONE',  ( -0.000000000000000000, -1.000000000000000000, -0.000000000000000000 ) ) ;
#5395 = LINE ( 'NONE', #6568, #5437 ) ;
#5396 = ADVANCED_FACE ( 'NONE', ( #1317 ), #2990, .F. ) ;
#5397 = CARTESIAN_POINT ( 'NONE',  ( 0.000000000000000000, 0.000000000000000000, -77.51594804401857175 ) ) ;
#5398 = CARTESIAN_POINT ( 'NONE',  ( 15.91624278015930649, 5.932232821383347954, -217.3600859879243217 ) ) ;
#5399 = CARTESIAN_POINT ( 'NONE',  ( -9.222253059793434460, 13.27185325399938165, -229.0864811363590547 ) ) ;
#5400 = CARTESIAN_POINT ( 'NONE',  ( 15.51445714770079931, 9.275596138242290678, -215.8565574371285436 ) ) ;
#5401 = CARTESIAN_POINT ( 'NONE',  ( -29.95012366401462955, 4.746560250930182967, -224.6954343660969471 ) ) ;
#5402 =( BOUNDED_SURFACE ( )  B_SPLINE_SURFACE ( 3, 3, ( 
 ( #7847, #7953, #2864, #14818, #8179, #1413, #11656, #21441, #15044, #21663, #6253, #20185, #4560, #9748, #18415, #9976, #16611, #14935, #21775, #6363, #13235, #4668, #21885, #14606, #5334, #57, #6931, #8623, #1853, #3311, #20300, #15154, #11775, #18853, #12217, #4895, #10196, #8404, #17279, #17172, #5111, #18639, #6591, #20753, #17064, #8285, #22228, #18962, #13579, #10525, #11993, #8731, #18744, #10084, #13460, #17395, #1641, #3428, #15271, #6819, #5226, #10308, #13918, #15598, #8518, #21996, #15381, #177, #10418, #3202, #13685, #7046, #16949, #19069, #22121, #3539, #20522, #5004, #3644, #6708, #1525, #20415, #11881, #1749, #15484, #13802, #20641, #12107, #15713, #7490, #19617, #17617, #5566, #14139, #9180, #15931, #2183, #14359, #17510, #21295, #12444, #20978, #9286, #9064, #15821, #508, #19182, #14025, #5777, #5445, #7159, #12327, #3758, #19294, #21085, #10751, #19504, #11081, #14462, #8847, #2405, #7384, #14252, #16147, #5672, #12550, #719, #5892, #2077, #290, #20862, #4094, #21192, #10643, #12658, #3871, #12769, #16043, #19397, #4202, #1969, #8957, #3980, #10854, #7593, #397, #7270, #17728, #2296, #10970, #17840, #615, #8039, #12981, #21857, #2839, #7925, #13316, #8152, #20157, #14907, #4750, #1052, #19724, #11298, #827, #11186, #21412, #16365, #17948, #15017, #9721, #16583, #18278, #11515, #19828, #7707, #2512, #6002, #6222, #6446, #14576, #4414, #18052, #4642, #4533, #14788, #12874, #16252, #9390, #18169, #4304, #9613, #6337, #942, #2621, #21630, #18385, #6110, #9504, #7819, #14684, #2733, #13098, #21518, #16475, #21747, #19944, #1278, #2948, #11409, #1164, #13210, #9835, #20055, #16697, #20389, #20613, #9952, #3513, #11749, #35, #17040, #8377, #1825, #3176, #16811, #18615, #10393, #17253, #16924, #15568, #8262, #5088, #3063, #17150, #7016, #4982, #15246, #1498, #18830, #3287, #11857, #1727, #4870, #8702, #22092, #6682, #18938, #18722, #10060, #10171, #6561, #1387, #15462, #15129, #21968, #13433, #20275, #13554, #8494, #1616, #6905, #20727, #148, #18502, #12082, #15358, #22205, #13890, #6794, #11629, #13662, #20498, #5199, #11968, #3404, #8601, #10285, #13774, #14439, #8930, #10831, #375, #7243, #14113, #17817, #9039, #2382, #483, #20949, #7133, #2159, #5537, #12526, #8820, #2052, #2270, #7573, #10613, #5417, #17484, #9266, #10945, #19481, #19375, #5307, #10499, #3847, #20835, #3956, #19267, #15905, #16123, #5754, #12415, #17364, #17703, #3731, #12300, #15797, #12189, #19153, #21061, #7358, #16015, #10727, #19044, #697, #5649, #17592, #3620, #14225, #9153, #592, #7465 ),
 ( #1940, #14333, #21167, #12634, #4069, #15685, #263, #13999, #11495, #7799, #21274, #12963, #9700, #4286, #1254, #2711, #21722, #9482, #806, #4182, #8129, #14664, #9594, #5982, #19807, #18257, #16457, #4620, #6315, #21497, #5865, #6087, #13189, #1139, #12746, #4391, #8017, #19593, #20033, #21390, #16560, #11276, #18032, #18363, #12857, #11058, #19699, #2924, #9811, #11165, #16674, #17926, #18145, #11389, #2490, #9370, #13077, #16230, #16342, #1030, #7906, #14881, #7685, #14554, #2601, #14767, #918, #21608, #6200, #2820, #19921, #4508, #1800, #18590, #20472, #10036, #16898, #1473, #5172, #18698, #12054, #10145, #8349, #16789, #11832, #15220, #22179, #18476, #11720, #11941, #17227, #20249, #15107, #4844, #18911, #20586, #6877, #6768, #14995, #20135, #13522, #8238, #13637, #6654, #3261, #3488, #15438, #22065, #4725, #5064, #13406, #21944, #3152, #21834, #6536, #8467, #17014, #3375, #20363, #6423, #10364, #15333, #4955, #13294, #1591, #18805, #10256, #17123, #13749, #11605, #3039, #9925, #1364, #1701, #8573, #8, #15986, #13862, #10585, #453, #20810, #17789, #9124, #19238, #12270, #8904, #7330, #15656, #8676, #21140, #15876, #4038, #15770, #3703, #14307, #19451, #5727, #5386, #563, #9011, #20920, #20702, #12607, #10917, #7106, #7439, #19123, #15540, #236, #123, #5280, #6990, #5509, #19017, #12161, #3594, #10471, #17334, #10701, #1913, #2024, #8795, #10805, #13970, #17455, #17671, #348, #7217, #14082, #19348, #12388, #3818, #17565, #2134, #14198, #21035, #5623, #12501, #3930, #2242, #21246, #18118, #16099, #7879, #20006, #18007, #5954, #14528, #9567, #16316, #2571, #14741, #17899, #21695, #12831, #21362, #9673, #9455, #16204, #892, #19565, #14414, #6169, #5838, #7545, #12718, #4152, #19674, #21470, #11139, #19893, #11467, #14851, #9239, #2790, #7768, #14638, #16532, #6062, #12936, #1111, #6286, #2462, #670, #11032, #4482, #21581, #9345, #13046, #4261, #13160, #16429, #19782, #4591, #2354, #776, #11361, #7656, #4363, #11246, #2685, #1004, #18230, #7986, #16760, #13722, #15415, #10119, #16984, #18674, #11915, #13378, #8101, #2897, #21808, #6626, #22259, #14968, #20220, #18448, #5038, #4931, #15191, #6396, #16645, #8551, #4816, #18336, #10009, #6744, #1339, #20561, #22035, #18781, #6508, #20111, #1227, #5148, #11694, #13497, #3011, #16872, #15307, #20335, #1677, #3347, #18564, #9780, #11807, #3235, #13267, #4699, #6854, #3129, #11574, #1449, #13612, #8210, #9896, #1563, #10230, #8321, #15082, #21918, #8437, #22155, #20449, #17099, #3679, #8992, #7195, #17652, #19329, #5367, #21120, #12251 ),
 ( #8771, #2217, #3575, #17206, #12140, #10784, #3908, #17313, #15966, #8655, #5483, #3464, #17545, #7418, #19102, #15633, #1888, #19216, #10563, #17433, #2113, #5260, #9099, #214, #7083, #539, #2003, #10452, #8885, #6968, #1780, #15855, #15516, #98, #13840, #20678, #13951, #15749, #20786, #7306, #12029, #14286, #18890, #12482, #327, #14062, #10342, #20897, #12367, #18995, #3798, #10682, #431, #14176, #21011, #5601, #10890, #14614, #17877, #8155, #9427, #5928, #21860, #1281, #6449, #21448, #13319, #21334, #16079, #16183, #4014, #7525, #2330, #5814, #5708, #15020, #7742, #6037, #16290, #18090, #9323, #17766, #19430, #9216, #4236, #12585, #12694, #19651, #2439, #648, #21226, #14394, #19541, #4129, #11010, #11116, #4338, #754, #14500, #7630, #12807, #17984, #2546, #865, #12911, #19758, #2952, #11222, #9840, #16701, #19388, #17383, #16033, #499, #5434, #9169, #12951, #7150, #9053, #20852, #12318, #19171, #606, #7258, #7480, #20967, #3748, #5325, #389, #10633, #10742, #7037, #280, #7374, #5767, #8837, #3636, #15703, #14350, #21182, #17719, #17607, #3529, #8721, #2067, #19061, #2174, #17500, #14130, #10409, #3971, #8947, #15588, #15921, #1958, #10517, #14015, #17270, #15813, #19284, #5554, #14242, #12434, #1843, #166, #3861, #21075, #13908, #5663, #12541, #10844, #2284, #20744, #12206, #15207, #9581, #11708, #1125, #22053, #8336, #4832, #2699, #21710, #11591, #9687, #6642, #20237, #8117, #8002, #20020, #18464, #4498, #19795, #10024, #4712, #4378, #4607, #14868, #3141, #11263, #16886, #16547, #18579, #20124, #9796, #16444, #1461, #18132, #18245, #1017, #6302, #7893, #11377, #14754, #18349, #3027, #1243, #21595, #6186, #13282, #13064, #9914, #19909, #13176, #11482, #2911, #16777, #16661, #14982, #1353, #2807, #21822, #6412, #8225, #15096, #21933, #6523, #13393, #9951, #16810, #18384, #13432, #1386, #1496, #20054, #13315, #13553, #18829, #21856, #16695, #6445, #13661, #22204, #8493, #8376, #3402, #21746, #15128, #9834, #15245, #8261, #4869, #5086, #17039, #11628, #6336, #22090, #15016, #1277, #20156, #16582, #8151, #10059, #20273, #4981, #4749, #1163, #11967, #16923, #18500, #8038, #11748, #3175, #18614, #6681, #15357, #20497, #14905, #13209, #6793, #3062, #4641, #11514, #1614, #2947, #21967, #20388, #6560, #11856, #18721, #3285, #10170, #10497, #8929, #17252, #10284, #482, #17483, #5648, #17363, #5306, #15903, #21060, #7357, #7015, #17591, #10612, #262, #15461, #14224, #12525, #8700, #9038, #20726, #19374, #1824, #1726, #8819, #15796, #13998, #17149, #8600, #34, #6903, #13773, #12298 ),
 ( #7242, #12188, #20612, #5197, #13889, #374, #19043, #3619, #1939, #12081, #18937, #15567, #15684, #7132, #3512, #20834, #5416, #2051, #10392, #19152, #14111, #147, #3730, #20948, #5536, #12414, #19266, #2158, #3846, #10726, #9152, #2489, #19479, #11164, #17925, #14553, #14766, #4390, #21273, #16014, #9481, #2381, #4068, #16122, #6199, #10944, #19698, #7684, #14663, #9265, #3955, #21607, #4285, #696, #10830, #21389, #12856, #5981, #2600, #2710, #7905, #13076, #591, #18144, #7572, #17701, #2269, #11275, #7464, #5864, #18031, #14438, #14332, #9593, #16341, #12745, #4181, #917, #17816, #21166, #16456, #7798, #5753, #11057, #19592, #1029, #12633, #9369, #16229, #805, #21496, #6086, #12962, #19806, #22178, #18362, #18697, #8128, #3260, #4619, #11388, #18475, #3151, #1363, #6767, #18256, #19920, #10144, #8466, #21943, #8016, #6422, #10035, #4507, #2819, #11719, #15332, #14994, #3038, #9924, #22064, #9699, #1590, #13188, #15106, #13521, #11494, #17013, #16559, #1138, #6653, #16897, #14880, #1472, #21833, #21721, #4843, #16788, #6314, #20032, #2923, #8348, #9810, #8237, #16673, #13293, #1253, #20134, #4724, #11604, #6535, #13405, #18589, #15219, #20248, #20362, #4954, #11831, #20471, #17122, #1912, #17564, #10255, #8675, #13748, #347, #235, #10470, #1700, #11940, #3817, #122, #13636, #5279, #2023, #18910, #15875, #17333, #14081, #1799, #15437, #18804, #452, #6989, #8794, #20585, #12160, #10584, #15655, #19237, #20919, #13861, #5063, #20701, #5508, #7105, #12387, #13969, #2133, #3374, #10700, #5171, #8903, #19016, #10363, #9010, #12053, #8572, #3487, #7, #6876, #17226, #15539, #3593, #20809, #5385, #19122, #12269, #3702, #17454, #15769, #7216, #21245, #7544, #12830, #562, #4362, #10916, #19450, #14637, #14413, #9238, #11138, #19781, #21361, #18006, #10804, #12500, #17670, #2241, #4037, #4151, #16098, #2570, #16428, #11245, #14197, #7767, #5837, #12717, #21469, #19564, #17898, #6061, #18117, #7438, #19673, #2684, #669, #17788, #2353, #14527, #11031, #2461, #4260, #14306, #9566, #9344, #16203, #12935, #775, #7655, #9454, #7329, #5953, #16315, #9123, #19347, #15985, #21139, #891, #21034, #5622, #3929, #5726, #12606, #7878, #1448, #8100, #14967, #15190, #13266, #11573, #22034, #13496, #1110, #14740, #21580, #3128, #6507, #13045, #13377, #18335, #4930, #8209, #20110, #18673, #20334, #3234, #20219, #10118, #6395, #2789, #16644, #6168, #16531, #4481, #21694, #1003, #11806, #15081, #21917, #1338, #16871, #2896, #19892, #11360, #18229, #18447, #9672, #7985, #9779, #14850, #10008, #9895, #4698 ),
 ( #8320, #11466, #6285, #13159, #20005, #1226, #3010, #4590, #21807, #4815, #16759, #6625, #11693, #18563, #3797, #10341, #8884, #12139, #15748, #20677, #20896, #15306, #326, #17098, #5366, #97, #13721, #7194, #8550, #22154, #1676, #14061, #5482, #22258, #12366, #13611, #10451, #8436, #19215, #16983, #6853, #1562, #20448, #17312, #6743, #213, #5037, #17205, #20560, #5147, #1887, #8654, #1779, #7082, #10229, #11914, #12028, #18889, #2002, #15515, #3463, #20785, #18780, #8770, #12250, #3346, #15414, #6967, #13839, #5259, #18994, #3574, #19101, #15632, #13950, #3678, #17432, #10562, #17765, #2545, #647, #21225, #9426, #864, #10783, #17544, #8991, #12806, #16182, #430, #753, #5707, #14613, #17876, #7524, #6036, #7741, #12910, #7629, #19757, #16078, #12481, #4013, #15854, #3907, #14175, #9098, #10681, #21447, #2438, #9322, #11009, #4235, #12584, #7305, #2112, #21010, #5813, #5600, #19328, #19429, #17651, #19650, #19540, #14393, #2216, #15965, #538, #10889, #7417, #2329, #21333, #14285, #21119, #12693, #11115, #9215, #4128, #14499, #5927, #17983, #16289, #11333, #18311, #1310, #21782, #9982, #11662, #19980, #13466, #4567, #18532, #6369, #3100, #8076, #8292, #2658, #16843, #4451, #15050, #9753, #1085, #1419, #18204, #9540, #2765, #7959, #16508, #11548, #2871, #11442, #9867, #19865, #15160, #14824, #21669, #22003, #16617, #6259, #8184, #6598, #18420, #21891, #7853, #16401, #14719, #21554, #13134, #1199, #14941, #6480, #4337, #11221, #18089, #4787, #13241, #20086, #978, #4673, #2984, #6145, #13019, #9646, #16732, #13349, #20192, #3545, #10090, #10423, #15387, #1973, #5231, #10315, #15718, #10532, #295, #17284, #7163, #3434, #22127, #13691, #3208, #13585, #1532, #18749, #20305, #17399, #12112, #18968, #20648, #13922, #22234, #16955, #4902, #8410, #8629, #8851, #15278, #6825, #20421, #7052, #6938, #17178, #6715, #18645, #11781, #20529, #5010, #12000, #8738, #3319, #11887, #1754, #20757, #8523, #10202, #17069, #1648, #5118, #15489, #18859, #64, #1859, #13808, #3648, #5338, #15604, #182, #12221, #19073, #9185, #5899, #17736, #17954, #12334, #12775, #14146, #2411, #19402, #10757, #4208, #5571, #19187, #20983, #19623, #11087, #19299, #2518, #10648, #7495, #5451, #19512, #9396, #7389, #3876, #834, #14468, #2301, #17622, #14258, #12664, #12448, #14030, #16258, #21197, #20866, #21091, #9069, #3763, #17515, #2083, #2188, #21302, #14364, #3985, #8961, #15825, #402, #15938, #7276, #513, #5677, #12555, #10860, #16048, #4099, #619, #5785, #10977, #17847, #9293, #16154, #725, #7600, #16480, #20368 ),
 ( #13530, #3380, #1057, #11303, #19833, #15225, #21635, #7930, #4959, #948, #5069, #18174, #4421, #15338, #14793, #9618, #11838, #20478, #22069, #18703, #11192, #12880, #18058, #2629, #2738, #4538, #6229, #3266, #17129, #11945, #14583, #8471, #13103, #19949, #22185, #11726, #18594, #6773, #18809, #7824, #21418, #6008, #10150, #17019, #19730, #1594, #3157, #10261, #6659, #10041, #7713, #4310, #9510, #13642, #16371, #16902, #14689, #1478, #21523, #6115, #12986, #8354, #19353, #21039, #15775, #354, #2030, #17570, #19021, #13752, #8579, #5177, #12276, #5628, #20591, #3599, #1804, #15547, #14203, #20927, #10475, #7336, #10810, #5285, #7222, #17340, #1918, #8799, #6883, #3493, #126, #15660, #241, #10369, #20814, #7110, #8909, #12059, #20707, #5514, #3935, #6994, #8681, #13866, #12506, #1705, #15881, #14087, #15443, #18917, #13974, #17233, #12393, #5391, #19128, #13, #2139, #3708, #12165, #19243, #10590, #17460, #3824, #10706, #9016, #459, #21366, #6068, #674, #17677, #13054, #11143, #16103, #2249, #12835, #4265, #19679, #16320, #16433, #21586, #19899, #7444, #9571, #21251, #4487, #6175, #2689, #568, #19569, #9460, #7550, #9129, #18122, #5958, #5843, #17903, #896, #2359, #15992, #7883, #2577, #14311, #2467, #12722, #1008, #21144, #14745, #14418, #5731, #18011, #7662, #12611, #19456, #4044, #4156, #10921, #11037, #17793, #9243, #9349, #16209, #7773, #14643, #781, #14532, #21474, #12940, #19785, #4368, #11252, #20114, #1453, #18235, #20455, #3133, #6749, #21813, #16765, #1344, #13503, #9678, #15313, #4596, #6513, #4936, #13617, #8215, #13165, #4703, #16537, #11472, #14857, #9786, #11366, #8444, #10014, #16878, #11699, #11812, #6402, #1116, #2795, #21700, #21923, #22160, #7992, #13272, #18340, #20340, #20227, #15087, #6291, #20010, #1571, #11580, #2901, #3017, #22043, #16651, #1232, #13383, #18679, #18454, #8106, #14972, #9902, #4822, #18569, #8326, #15196, #6632, #3241, #16990, #10125, #20682, #14181, #5264, #19222, #219, #3802, #8778, #8996, #3354, #10686, #5154, #15753, #10456, #1784, #17550, #18894, #10236, #12034, #2117, #15859, #10347, #436, #1682, #20791, #18786, #10568, #7310, #12144, #8659, #17210, #12255, #19000, #3579, #17438, #20566, #5043, #15520, #103, #12372, #17317, #6974, #8889, #11920, #19106, #332, #8556, #17103, #15420, #22263, #13845, #1893, #15639, #7200, #6858, #13726, #3469, #5488, #7088, #13955, #5371, #3683, #2007, #14066, #20902, #21124, #5605, #19333, #869, #4240, #10789, #11120, #16083, #2662, #5933, #11014, #16406, #11226, #982, #17988, #7857, #19762, #9546 ),
 ( #21018, #17656, #14504, #12486, #2550, #3913, #14398, #2336, #10895, #12811, #12699, #21230, #9434, #14291, #18095, #9220, #17770, #6041, #5820, #652, #16294, #2223, #19655, #7748, #9104, #15971, #545, #7422, #7530, #17882, #19545, #14618, #5712, #12589, #19434, #21452, #4135, #2444, #12916, #9327, #16187, #4342, #4019, #759, #7635, #21338, #16848, #20196, #4457, #4791, #9757, #18651, #21895, #4677, #10095, #4906, #16959, #11666, #1536, #20090, #16512, #8080, #19871, #7963, #18209, #13140, #14723, #11785, #6483, #13353, #15055, #8298, #16622, #11339, #21559, #2770, #2988, #3212, #9651, #1203, #14829, #1424, #1315, #11552, #1089, #13024, #6149, #14948, #21673, #6373, #3104, #19984, #6264, #18424, #15164, #2875, #4571, #11447, #18315, #21786, #9871, #13245, #16737, #18538, #8188, #20310, #22006, #9987, #6602, #13470, #299, #3550, #7169, #12116, #12338, #14034, #187, #10654, #13589, #6942, #1653, #15608, #69, #18971, #19191, #8858, #3439, #20427, #13926, #6830, #8527, #20533, #17520, #15391, #1863, #10427, #19077, #13697, #8414, #3768, #8743, #5123, #15282, #17288, #7058, #20761, #5343, #20870, #22131, #6719, #5015, #5455, #12004, #11891, #18754, #15722, #3323, #10319, #12225, #18863, #10206, #17073, #3652, #17182, #8633, #10536, #22239, #1759, #15493, #17404, #13813, #20652, #5235, #1977, #12884, #21423, #21096, #9400, #2415, #14368, #7280, #6012, #4314, #517, #838, #12560, #7717, #9073, #15830, #624, #7605, #5789, #11197, #406, #2087, #14587, #19734, #4103, #12455, #10865, #14473, #8965, #14150, #16159, #20987, #19406, #7500, #21202, #4212, #5575, #19303, #17626, #19517, #17958, #15941, #3881, #21306, #3989, #10761, #2193, #5681, #5903, #17740, #2305, #9189, #7393, #14263, #16053, #12669, #10981, #17852, #9297, #729, #12779, #19628, #11091, #2523, #16264, #1061, #18178, #7934, #15135, #1394, #9958, #21640, #13441, #6570, #3070, #953, #19954, #9845, #14798, #4876, #18508, #6346, #6234, #18286, #16706, #2742, #18062, #8268, #2959, #20281, #2847, #13107, #21976, #2634, #9514, #4542, #16817, #18394, #8049, #7828, #16374, #14693, #16484, #21528, #11418, #6118, #9622, #12990, #16592, #1286, #21755, #19839, #4425, #11308, #9729, #1174, #20063, #14916, #13218, #8160, #4650, #11524, #15026, #21865, #6455, #13324, #20166, #4760, #11637, #15689, #4986, #6910, #5311, #3291, #1945, #8707, #13666, #17370, #20839, #15363, #17257, #6799, #20502, #5093, #16930, #13561, #10176, #11974, #18835, #20395, #8605, #3409, #18942, #15253, #8498, #15574, #14003, #17045, #11861, #1621, #8824, #267, #3624 ) ),
 .UNSPECIFIED., .T., .F., .F. ) 
 B_SPLINE_SURFACE_WITH_KNOTS ( ( 4, 3, 4 ),
 ( 4, 2, 2, 2, 2, 2, 2, 2, 2, 2, 2, 2, 2, 2, 2, 2, 2, 2, 2, 2, 2, 2, 2, 2, 2, 2, 2, 2, 2, 2, 2, 2, 2, 2, 2, 2, 2, 2, 2, 2, 2, 2, 2, 2, 2, 2, 2, 2, 2, 2, 2, 2, 2, 2, 2, 2, 2, 2, 2, 2, 2, 2, 2, 2, 2, 2, 2, 2, 2, 2, 2, 2, 2, 2, 2, 2, 2, 2, 2, 2, 2, 2, 2, 2, 2, 2, 2, 2, 2, 2, 2, 2, 2, 2, 2, 2, 2, 2, 2, 2, 2, 2, 2, 2, 2, 2, 2, 2, 2, 2, 2, 2, 2, 2, 2, 2, 2, 2, 2, 2, 2, 2, 2, 2, 2, 2, 2, 2, 2, 2, 2, 2, 2, 2, 2, 2, 2, 2, 2, 2, 2, 2, 2, 2, 2, 2, 2, 2, 2, 2, 2, 2, 2, 2, 2, 2, 2, 2, 2, 2, 2, 2, 2, 2, 2, 2, 2, 4 ),
 ( 0.000000000000000000, 0.5000000000000000000, 1.000000000000000000 ),
 ( 0.000000000000000000, 0.001952908952989333875, 0.003905817905978667751, 0.007323408573709997045, 0.01074099924144132634, 0.01415858990917265650, 0.01586738524303832332, 0.01757618057690398666, 0.02099377124463531682, 0.02441136191236664699, 0.02782895258009797368, 0.03124654324782930384, 0.03466413391556063400, 0.03808172458329196070, 0.04149931525102329433, 0.04491690591875462102, 0.04662570125262028436, 0.04833449658648594771, 0.05175208725421727440, 0.05346088258808293775, 0.05516967792194860110, 0.05858726858967993473, 0.06200485925741126836, 0.06542244992514259505, 0.06884004059287393562, 0.07225763126060526231, 0.07567522192833658901, 0.07909281259606792958, 0.08251040326379925627, 0.08421919859766491268, 0.08592799393153058296, 0.08934558459926195129, 0.09276317526699331961, 0.09447197060085900377, 0.09618076593472468794, 0.09959835660245604239, 0.1030159472701873968, 0.1064335379379187652, 0.1098511286056501335, 0.1132687192733815018, 0.1166863099411127869, 0.1201039006088440858, 0.1235214912765753847, 0.1252302866104410273, 0.1269390819443066698, 0.1303566726120379826, 0.1320654679459036251, 0.1337742632797692677, 0.1371918539475005527, 0.1406094446152318378, 0.1440270352829631784, 0.1474446259506944912, 0.1508622166184258040, 0.1542798072861571446, 0.1576973979538884851, 0.1611149886216198257, 0.1645325792893511663, 0.1679501699570824791, 0.1713677606248137919, 0.1747853512925451325, 0.1764941466264108028, 0.1782029419602764730, 0.1816205326280078136, 0.1850381232957391542, 0.1884557139634704670, 0.1918733046312017798, 0.1952908952989331204, 0.1987084859666644610, 0.2021260766343957738, 0.2055436673021270866, 0.2072524626359927569, 0.2089612579698584272, 0.2123788486375897677, 0.2140876439714554380, 0.2157964393053211083, 0.2192140299730524489, 0.2226316206407837617, 0.2260492113085151300, 0.2294668019762464706, 0.2328843926439778111, 0.2363019833117091517, 0.2397195739794404923, 0.2431371646471718329, 0.2465547553149031734, 0.2499723459826345140, 0.2533899366503657991, 0.2568075273180971396, 0.2602251179858284802, 0.2636427086535597653, 0.2670602993212910503, 0.2704778899890223909, 0.2738954806567537315, 0.2773130713244850165, 0.2807306619922163571, 0.2841482526599476977, 0.2858570479938133957, 0.2875658433276790382, 0.2909834339954103788, 0.2926922293292760768, 0.2944010246631417194, 0.2978186153308730599, 0.3012362059986043450, 0.3046537966663356856, 0.3080713873340670261, 0.3114889780017983112, 0.3149065686695296518, 0.3183241593372609923, 0.3217417500049923329, 0.3234505453388579754, 0.3251593406727236735, 0.3285769313404549585, 0.3319945220081862991, 0.3354121126759176397, 0.3388297033436489247, 0.3422472940113802653, 0.3456648846791116059, 0.3490824753468429464, 0.3525000660145742870, 0.3559176566823056276, 0.3593352473500369682, 0.3627528380177683087, 0.3661704286854996493, 0.3695880193532309343, 0.3730056100209622749, 0.3747144053548279174, 0.3764232006886936155, 0.3798407913564249005, 0.3832583820241562411, 0.3866759726918875817, 0.3900935633596189223, 0.3935111540273502628, 0.3969287446950816034, 0.4003463353628129440, 0.4037639260305442845, 0.4054727213644099271, 0.4071815166982756251, 0.4105991073660069102, 0.4140166980337382507, 0.4157254933676038933, 0.4174342887014695913, 0.4208518793692008764, 0.4242694700369322169, 0.4276870607046635575, 0.4311046513723948981, 0.4345222420401262386, 0.4379398327078575237, 0.4413574233755888643, 0.4447750140433202048, 0.4464838093771859029, 0.4481926047110515454, 0.4516101953787828860, 0.4533189907126485840, 0.4550277860465142266, 0.4584453767142455671, 0.4618629673819769077, 0.4652805580497082483, 0.4686981487174395888, 0.4721157393851709294, 0.4755333300529022145, 0.4789509207206335550, 0.4823685113883648956, 0.4840773067222305381, 0.4857861020560961807, 0.4892036927238275212, 0.4926212833915588618, 0.4960388740592901469, 0.4979917830122794764, 0.4999446919652688059 ),
 .UNSPECIFIED. ) 
 GEOMETRIC_REPRESENTATION_ITEM ( )  RATIONAL_B_SPLINE_SURFACE ( (
 ( 1.000000000000000000, 1.000000000000000000, 1.000000000000000000, 1.000000000000000000, 1.000000000000000000, 1.000000000000000000, 1.000000000000000000, 1.000000000000000000, 1.000000000000000000, 1.000000000000000000, 1.000000000000000000, 1.000000000000000000, 1.000000000000000000, 1.000000000000000000, 1.000000000000000000, 1.000000000000000000, 1.000000000000000000, 1.000000000000000000, 1.000000000000000000, 1.000000000000000000, 1.000000000000000000, 1.000000000000000000, 1.000000000000000000, 1.000000000000000000, 1.000000000000000000, 1.000000000000000000, 1.000000000000000000, 1.000000000000000000, 1.000000000000000000, 1.000000000000000000, 1.000000000000000000, 1.000000000000000000, 1.000000000000000000, 1.000000000000000000, 1.000000000000000000, 1.000000000000000000, 1.000000000000000000, 1.000000000000000000, 1.000000000000000000, 1.000000000000000000, 1.000000000000000000, 1.000000000000000000, 1.000000000000000000, 1.000000000000000000, 1.000000000000000000, 1.000000000000000000, 1.000000000000000000, 1.000000000000000000, 1.000000000000000000, 1.000000000000000000, 1.000000000000000000, 1.000000000000000000, 1.000000000000000000, 1.000000000000000000, 1.000000000000000000, 1.000000000000000000, 1.000000000000000000, 1.000000000000000000, 1.000000000000000000, 1.000000000000000000, 1.000000000000000000, 1.000000000000000000, 1.000000000000000000, 1.000000000000000000, 1.000000000000000000, 1.000000000000000000, 1.000000000000000000, 1.000000000000000000, 1.000000000000000000, 1.000000000000000000, 1.000000000000000000, 1.000000000000000000, 1.000000000000000000, 1.000000000000000000, 1.000000000000000000, 1.000000000000000000, 1.000000000000000000, 1.000000000000000000, 1.000000000000000000, 1.000000000000000000, 1.000000000000000000, 1.000000000000000000, 1.000000000000000000, 1.000000000000000000, 1.000000000000000000, 1.000000000000000000, 1.000000000000000000, 1.000000000000000000, 1.000000000000000000, 1.000000000000000000, 1.000000000000000000, 1.000000000000000000, 1.000000000000000000, 1.000000000000000000, 1.000000000000000000, 1.000000000000000000, 1.000000000000000000, 1.000000000000000000, 1.000000000000000000, 1.000000000000000000, 1.000000000000000000, 1.000000000000000000, 1.000000000000000000, 1.000000000000000000, 1.000000000000000000, 1.000000000000000000, 1.000000000000000000, 1.000000000000000000, 1.000000000000000000, 1.000000000000000000, 1.000000000000000000, 1.000000000000000000, 1.000000000000000000, 1.000000000000000000, 1.000000000000000000, 1.000000000000000000, 1.000000000000000000, 1.000000000000000000, 1.000000000000000000, 1.000000000000000000, 1.000000000000000000, 1.000000000000000000, 1.000000000000000000, 1.000000000000000000, 1.000000000000000000, 1.000000000000000000, 1.000000000000000000, 1.000000000000000000, 1.000000000000000000, 1.000000000000000000, 1.000000000000000000, 1.000000000000000000, 1.000000000000000000, 1.000000000000000000, 1.000000000000000000, 1.000000000000000000, 1.000000000000000000, 1.000000000000000000, 1.000000000000000000, 1.000000000000000000, 1.000000000000000000, 1.000000000000000000, 1.000000000000000000, 1.000000000000000000, 1.000000000000000000, 1.000000000000000000, 1.000000000000000000, 1.000000000000000000, 1.000000000000000000, 1.000000000000000000, 1.000000000000000000, 1.000000000000000000, 1.000000000000000000, 1.000000000000000000, 1.000000000000000000, 1.000000000000000000, 1.000000000000000000, 1.000000000000000000, 1.000000000000000000, 1.000000000000000000, 1.000000000000000000, 1.000000000000000000, 1.000000000000000000, 1.000000000000000000, 1.000000000000000000, 1.000000000000000000, 1.000000000000000000, 1.000000000000000000, 1.000000000000000000, 1.000000000000000000, 1.000000000000000000, 1.000000000000000000, 1.000000000000000000, 1.000000000000000000, 1.000000000000000000, 1.000000000000000000, 1.000000000000000000, 1.000000000000000000, 1.000000000000000000, 1.000000000000000000, 1.000000000000000000, 1.000000000000000000, 1.000000000000000000, 1.000000000000000000, 1.000000000000000000, 1.000000000000000000, 1.000000000000000000, 1.000000000000000000, 1.000000000000000000, 1.000000000000000000, 1.000000000000000000, 1.000000000000000000, 1.000000000000000000, 1.000000000000000000, 1.000000000000000000, 1.000000000000000000, 1.000000000000000000, 1.000000000000000000, 1.000000000000000000, 1.000000000000000000, 1.000000000000000000, 1.000000000000000000, 1.000000000000000000, 1.000000000000000000, 1.000000000000000000, 1.000000000000000000, 1.000000000000000000, 1.000000000000000000, 1.000000000000000000, 1.000000000000000000, 1.000000000000000000, 1.000000000000000000, 1.000000000000000000, 1.000000000000000000, 1.000000000000000000, 1.000000000000000000, 1.000000000000000000, 1.000000000000000000, 1.000000000000000000, 1.000000000000000000, 1.000000000000000000, 1.000000000000000000, 1.000000000000000000, 1.000000000000000000, 1.000000000000000000, 1.000000000000000000, 1.000000000000000000, 1.000000000000000000, 1.000000000000000000, 1.000000000000000000, 1.000000000000000000, 1.000000000000000000, 1.000000000000000000, 1.000000000000000000, 1.000000000000000000, 1.000000000000000000, 1.000000000000000000, 1.000000000000000000, 1.000000000000000000, 1.000000000000000000, 1.000000000000000000, 1.000000000000000000, 1.000000000000000000, 1.000000000000000000, 1.000000000000000000, 1.000000000000000000, 1.000000000000000000, 1.000000000000000000, 1.000000000000000000, 1.000000000000000000, 1.000000000000000000, 1.000000000000000000, 1.000000000000000000, 1.000000000000000000, 1.000000000000000000, 1.000000000000000000, 1.000000000000000000, 1.000000000000000000, 1.000000000000000000, 1.000000000000000000, 1.000000000000000000, 1.000000000000000000, 1.000000000000000000, 1.000000000000000000, 1.000000000000000000, 1.000000000000000000, 1.000000000000000000, 1.000000000000000000, 1.000000000000000000, 1.000000000000000000, 1.000000000000000000, 1.000000000000000000, 1.000000000000000000, 1.000000000000000000, 1.000000000000000000, 1.000000000000000000, 1.000000000000000000, 1.000000000000000000, 1.000000000000000000, 1.000000000000000000, 1.000000000000000000, 1.000000000000000000, 1.000000000000000000, 1.000000000000000000, 1.000000000000000000, 1.000000000000000000, 1.000000000000000000, 1.000000000000000000, 1.000000000000000000, 1.000000000000000000, 1.000000000000000000, 1.000000000000000000, 1.000000000000000000, 1.000000000000000000, 1.000000000000000000, 1.000000000000000000, 1.000000000000000000, 1.000000000000000000, 1.000000000000000000, 1.000000000000000000, 1.000000000000000000, 1.000000000000000000, 1.000000000000000000, 1.000000000000000000, 1.000000000000000000, 1.000000000000000000, 1.000000000000000000, 1.000000000000000000, 1.000000000000000000, 1.000000000000000000, 1.000000000000000000, 1.000000000000000000, 1.000000000000000000, 1.000000000000000000, 1.000000000000000000, 1.000000000000000000, 1.000000000000000000, 1.000000000000000000, 1.000000000000000000, 1.000000000000000000, 1.000000000000000000, 1.000000000000000000, 1.000000000000000000, 1.000000000000000000, 1.000000000000000000, 1.000000000000000000, 1.000000000000000000, 1.000000000000000000, 1.000000000000000000, 1.000000000000000000, 1.000000000000000000, 1.000000000000000000, 1.000000000000000000, 1.000000000000000000, 1.000000000000000000, 1.000000000000000000),
 ( 0.3333333333333333703, 0.3333333333333333703, 0.3333333333333333703, 0.3333333333333333703, 0.3333333333333333703, 0.3333333333333333703, 0.3333333333333333703, 0.3333333333333333703, 0.3333333333333333703, 0.3333333333333333703, 0.3333333333333333703, 0.3333333333333333703, 0.3333333333333333703, 0.3333333333333333703, 0.3333333333333333703, 0.3333333333333333703, 0.3333333333333333703, 0.3333333333333333703, 0.3333333333333333703, 0.3333333333333333703, 0.3333333333333333703, 0.3333333333333333703, 0.3333333333333333703, 0.3333333333333333703, 0.3333333333333333703, 0.3333333333333333703, 0.3333333333333333703, 0.3333333333333333703, 0.3333333333333333703, 0.3333333333333333703, 0.3333333333333333703, 0.3333333333333333703, 0.3333333333333333703, 0.3333333333333333703, 0.3333333333333333703, 0.3333333333333333703, 0.3333333333333333703, 0.3333333333333333703, 0.3333333333333333703, 0.3333333333333333703, 0.3333333333333333703, 0.3333333333333333703, 0.3333333333333333703, 0.3333333333333333703, 0.3333333333333333703, 0.3333333333333333703, 0.3333333333333333703, 0.3333333333333333703, 0.3333333333333333703, 0.3333333333333333703, 0.3333333333333333703, 0.3333333333333333703, 0.3333333333333333703, 0.3333333333333333703, 0.3333333333333333703, 0.3333333333333333703, 0.3333333333333333703, 0.3333333333333333703, 0.3333333333333333703, 0.3333333333333333703, 0.3333333333333333703, 0.3333333333333333703, 0.3333333333333333703, 0.3333333333333333703, 0.3333333333333333703, 0.3333333333333333703, 0.3333333333333333703, 0.3333333333333333703, 0.3333333333333333703, 0.3333333333333333703, 0.3333333333333333703, 0.3333333333333333703, 0.3333333333333333703, 0.3333333333333333703, 0.3333333333333333703, 0.3333333333333333703, 0.3333333333333333703, 0.3333333333333333703, 0.3333333333333333703, 0.3333333333333333703, 0.3333333333333333703, 0.3333333333333333703, 0.3333333333333333703, 0.3333333333333333703, 0.3333333333333333703, 0.3333333333333333703, 0.3333333333333333703, 0.3333333333333333703, 0.3333333333333333703, 0.3333333333333333703, 0.3333333333333333703, 0.3333333333333333703, 0.3333333333333333703, 0.3333333333333333703, 0.3333333333333333703, 0.3333333333333333703, 0.3333333333333333703, 0.3333333333333333703, 0.3333333333333333703, 0.3333333333333333703, 0.3333333333333333703, 0.3333333333333333703, 0.3333333333333333703, 0.3333333333333333703, 0.3333333333333333703, 0.3333333333333333703, 0.3333333333333333703, 0.3333333333333333703, 0.3333333333333333703, 0.3333333333333333703, 0.3333333333333333703, 0.3333333333333333703, 0.3333333333333333703, 0.3333333333333333703, 0.3333333333333333703, 0.3333333333333333703, 0.3333333333333333703, 0.3333333333333333703, 0.3333333333333333703, 0.3333333333333333703, 0.3333333333333333703, 0.3333333333333333703, 0.3333333333333333703, 0.3333333333333333703, 0.3333333333333333703, 0.3333333333333333703, 0.3333333333333333703, 0.3333333333333333703, 0.3333333333333333703, 0.3333333333333333703, 0.3333333333333333703, 0.3333333333333333703, 0.3333333333333333703, 0.3333333333333333703, 0.3333333333333333703, 0.3333333333333333703, 0.3333333333333333703, 0.3333333333333333703, 0.3333333333333333703, 0.3333333333333333703, 0.3333333333333333703, 0.3333333333333333703, 0.3333333333333333703, 0.3333333333333333703, 0.3333333333333333703, 0.3333333333333333703, 0.3333333333333333703, 0.3333333333333333703, 0.3333333333333333703, 0.3333333333333333703, 0.3333333333333333703, 0.3333333333333333703, 0.3333333333333333703, 0.3333333333333333703, 0.3333333333333333703, 0.3333333333333333703, 0.3333333333333333703, 0.3333333333333333703, 0.3333333333333333703, 0.3333333333333333703, 0.3333333333333333703, 0.3333333333333333703, 0.3333333333333333703, 0.3333333333333333703, 0.3333333333333333703, 0.3333333333333333703, 0.3333333333333333703, 0.3333333333333333703, 0.3333333333333333703, 0.3333333333333333703, 0.3333333333333333703, 0.3333333333333333703, 0.3333333333333333703, 0.3333333333333333703, 0.3333333333333333703, 0.3333333333333333703, 0.3333333333333333703, 0.3333333333333333703, 0.3333333333333333703, 0.3333333333333333703, 0.3333333333333333703, 0.3333333333333333703, 0.3333333333333333703, 0.3333333333333333703, 0.3333333333333333703, 0.3333333333333333703, 0.3333333333333333703, 0.3333333333333333703, 0.3333333333333333703, 0.3333333333333333703, 0.3333333333333333703, 0.3333333333333333703, 0.3333333333333333703, 0.3333333333333333703, 0.3333333333333333703, 0.3333333333333333703, 0.3333333333333333703, 0.3333333333333333703, 0.3333333333333333703, 0.3333333333333333703, 0.3333333333333333703, 0.3333333333333333703, 0.3333333333333333703, 0.3333333333333333703, 0.3333333333333333703, 0.3333333333333333703, 0.3333333333333333703, 0.3333333333333333703, 0.3333333333333333703, 0.3333333333333333703, 0.3333333333333333703, 0.3333333333333333703, 0.3333333333333333703, 0.3333333333333333703, 0.3333333333333333703, 0.3333333333333333703, 0.3333333333333333703, 0.3333333333333333703, 0.3333333333333333703, 0.3333333333333333703, 0.3333333333333333703, 0.3333333333333333703, 0.3333333333333333703, 0.3333333333333333703, 0.3333333333333333703, 0.3333333333333333703, 0.3333333333333333703, 0.3333333333333333703, 0.3333333333333333703, 0.3333333333333333703, 0.3333333333333333703, 0.3333333333333333703, 0.3333333333333333703, 0.3333333333333333703, 0.3333333333333333703, 0.3333333333333333703, 0.3333333333333333703, 0.3333333333333333703, 0.3333333333333333703, 0.3333333333333333703, 0.3333333333333333703, 0.3333333333333333703, 0.3333333333333333703, 0.3333333333333333703, 0.3333333333333333703, 0.3333333333333333703, 0.3333333333333333703, 0.3333333333333333703, 0.3333333333333333703, 0.3333333333333333703, 0.3333333333333333703, 0.3333333333333333703, 0.3333333333333333703, 0.3333333333333333703, 0.3333333333333333703, 0.3333333333333333703, 0.3333333333333333703, 0.3333333333333333703, 0.3333333333333333703, 0.3333333333333333703, 0.3333333333333333703, 0.3333333333333333703, 0.3333333333333333703, 0.3333333333333333703, 0.3333333333333333703, 0.3333333333333333703, 0.3333333333333333703, 0.3333333333333333703, 0.3333333333333333703, 0.3333333333333333703, 0.3333333333333333703, 0.3333333333333333703, 0.3333333333333333703, 0.3333333333333333703, 0.3333333333333333703, 0.3333333333333333703, 0.3333333333333333703, 0.3333333333333333703, 0.3333333333333333703, 0.3333333333333333703, 0.3333333333333333703, 0.3333333333333333703, 0.3333333333333333703, 0.3333333333333333703, 0.3333333333333333703, 0.3333333333333333703, 0.3333333333333333703, 0.3333333333333333703, 0.3333333333333333703, 0.3333333333333333703, 0.3333333333333333703, 0.3333333333333333703, 0.3333333333333333703, 0.3333333333333333703, 0.3333333333333333703, 0.3333333333333333703, 0.3333333333333333703, 0.3333333333333333703, 0.3333333333333333703, 0.3333333333333333703, 0.3333333333333333703, 0.3333333333333333703, 0.3333333333333333703, 0.3333333333333333703, 0.3333333333333333703, 0.3333333333333333703, 0.3333333333333333703, 0.3333333333333333703, 0.3333333333333333703, 0.3333333333333333703, 0.3333333333333333703, 0.3333333333333333703, 0.3333333333333333703, 0.3333333333333333703, 0.3333333333333333703, 0.3333333333333333703, 0.3333333333333333703, 0.3333333333333333703, 0.3333333333333333703, 0.3333333333333333703, 0.3333333333333333703, 0.3333333333333333703, 0.3333333333333333703, 0.3333333333333333703, 0.3333333333333333703, 0.3333333333333333703, 0.3333333333333333703, 0.3333333333333333703, 0.3333333333333333703, 0.3333333333333333703, 0.3333333333333333703, 0.3333333333333333703, 0.3333333333333333703, 0.3333333333333333703, 0.3333333333333333703, 0.3333333333333333703),
 ( 0.3333333333333333703, 0.3333333333333333703, 0.3333333333333333703, 0.3333333333333333703, 0.3333333333333333703, 0.3333333333333333703, 0.3333333333333333703, 0.3333333333333333703, 0.3333333333333333703, 0.3333333333333333703, 0.3333333333333333703, 0.3333333333333333703, 0.3333333333333333703, 0.3333333333333333703, 0.3333333333333333703, 0.3333333333333333703, 0.3333333333333333703, 0.3333333333333333703, 0.3333333333333333703, 0.3333333333333333703, 0.3333333333333333703, 0.3333333333333333703, 0.3333333333333333703, 0.3333333333333333703, 0.3333333333333333703, 0.3333333333333333703, 0.3333333333333333703, 0.3333333333333333703, 0.3333333333333333703, 0.3333333333333333703, 0.3333333333333333703, 0.3333333333333333703, 0.3333333333333333703, 0.3333333333333333703, 0.3333333333333333703, 0.3333333333333333703, 0.3333333333333333703, 0.3333333333333333703, 0.3333333333333333703, 0.3333333333333333703, 0.3333333333333333703, 0.3333333333333333703, 0.3333333333333333703, 0.3333333333333333703, 0.3333333333333333703, 0.3333333333333333703, 0.3333333333333333703, 0.3333333333333333703, 0.3333333333333333703, 0.3333333333333333703, 0.3333333333333333703, 0.3333333333333333703, 0.3333333333333333703, 0.3333333333333333703, 0.3333333333333333703, 0.3333333333333333703, 0.3333333333333333703, 0.3333333333333333703, 0.3333333333333333703, 0.3333333333333333703, 0.3333333333333333703, 0.3333333333333333703, 0.3333333333333333703, 0.3333333333333333703, 0.3333333333333333703, 0.3333333333333333703, 0.3333333333333333703, 0.3333333333333333703, 0.3333333333333333703, 0.3333333333333333703, 0.3333333333333333703, 0.3333333333333333703, 0.3333333333333333703, 0.3333333333333333703, 0.3333333333333333703, 0.3333333333333333703, 0.3333333333333333703, 0.3333333333333333703, 0.3333333333333333703, 0.3333333333333333703, 0.3333333333333333703, 0.3333333333333333703, 0.3333333333333333703, 0.3333333333333333703, 0.3333333333333333703, 0.3333333333333333703, 0.3333333333333333703, 0.3333333333333333703, 0.3333333333333333703, 0.3333333333333333703, 0.3333333333333333703, 0.3333333333333333703, 0.3333333333333333703, 0.3333333333333333703, 0.3333333333333333703, 0.3333333333333333703, 0.3333333333333333703, 0.3333333333333333703, 0.3333333333333333703, 0.3333333333333333703, 0.3333333333333333703, 0.3333333333333333703, 0.3333333333333333703, 0.3333333333333333703, 0.3333333333333333703, 0.3333333333333333703, 0.3333333333333333703, 0.3333333333333333703, 0.3333333333333333703, 0.3333333333333333703, 0.3333333333333333703, 0.3333333333333333703, 0.3333333333333333703, 0.3333333333333333703, 0.3333333333333333703, 0.3333333333333333703, 0.3333333333333333703, 0.3333333333333333703, 0.3333333333333333703, 0.3333333333333333703, 0.3333333333333333703, 0.3333333333333333703, 0.3333333333333333703, 0.3333333333333333703, 0.3333333333333333703, 0.3333333333333333703, 0.3333333333333333703, 0.3333333333333333703, 0.3333333333333333703, 0.3333333333333333703, 0.3333333333333333703, 0.3333333333333333703, 0.3333333333333333703, 0.3333333333333333703, 0.3333333333333333703, 0.3333333333333333703, 0.3333333333333333703, 0.3333333333333333703, 0.3333333333333333703, 0.3333333333333333703, 0.3333333333333333703, 0.3333333333333333703, 0.3333333333333333703, 0.3333333333333333703, 0.3333333333333333703, 0.3333333333333333703, 0.3333333333333333703, 0.3333333333333333703, 0.3333333333333333703, 0.3333333333333333703, 0.3333333333333333703, 0.3333333333333333703, 0.3333333333333333703, 0.3333333333333333703, 0.3333333333333333703, 0.3333333333333333703, 0.3333333333333333703, 0.3333333333333333703, 0.3333333333333333703, 0.3333333333333333703, 0.3333333333333333703, 0.3333333333333333703, 0.3333333333333333703, 0.3333333333333333703, 0.3333333333333333703, 0.3333333333333333703, 0.3333333333333333703, 0.3333333333333333703, 0.3333333333333333703, 0.3333333333333333703, 0.3333333333333333703, 0.3333333333333333703, 0.3333333333333333703, 0.3333333333333333703, 0.3333333333333333703, 0.3333333333333333703, 0.3333333333333333703, 0.3333333333333333703, 0.3333333333333333703, 0.3333333333333333703, 0.3333333333333333703, 0.3333333333333333703, 0.3333333333333333703, 0.3333333333333333703, 0.3333333333333333703, 0.3333333333333333703, 0.3333333333333333703, 0.3333333333333333703, 0.3333333333333333703, 0.3333333333333333703, 0.3333333333333333703, 0.3333333333333333703, 0.3333333333333333703, 0.3333333333333333703, 0.3333333333333333703, 0.3333333333333333703, 0.3333333333333333703, 0.3333333333333333703, 0.3333333333333333703, 0.3333333333333333703, 0.3333333333333333703, 0.3333333333333333703, 0.3333333333333333703, 0.3333333333333333703, 0.3333333333333333703, 0.3333333333333333703, 0.3333333333333333703, 0.3333333333333333703, 0.3333333333333333703, 0.3333333333333333703, 0.3333333333333333703, 0.3333333333333333703, 0.3333333333333333703, 0.3333333333333333703, 0.3333333333333333703, 0.3333333333333333703, 0.3333333333333333703, 0.3333333333333333703, 0.3333333333333333703, 0.3333333333333333703, 0.3333333333333333703, 0.3333333333333333703, 0.3333333333333333703, 0.3333333333333333703, 0.3333333333333333703, 0.3333333333333333703, 0.3333333333333333703, 0.3333333333333333703, 0.3333333333333333703, 0.3333333333333333703, 0.3333333333333333703, 0.3333333333333333703, 0.3333333333333333703, 0.3333333333333333703, 0.3333333333333333703, 0.3333333333333333703, 0.3333333333333333703, 0.3333333333333333703, 0.3333333333333333703, 0.3333333333333333703, 0.3333333333333333703, 0.3333333333333333703, 0.3333333333333333703, 0.3333333333333333703, 0.3333333333333333703, 0.3333333333333333703, 0.3333333333333333703, 0.3333333333333333703, 0.3333333333333333703, 0.3333333333333333703, 0.3333333333333333703, 0.3333333333333333703, 0.3333333333333333703, 0.3333333333333333703, 0.3333333333333333703, 0.3333333333333333703, 0.3333333333333333703, 0.3333333333333333703, 0.3333333333333333703, 0.3333333333333333703, 0.3333333333333333703, 0.3333333333333333703, 0.3333333333333333703, 0.3333333333333333703, 0.3333333333333333703, 0.3333333333333333703, 0.3333333333333333703, 0.3333333333333333703, 0.3333333333333333703, 0.3333333333333333703, 0.3333333333333333703, 0.3333333333333333703, 0.3333333333333333703, 0.3333333333333333703, 0.3333333333333333703, 0.3333333333333333703, 0.3333333333333333703, 0.3333333333333333703, 0.3333333333333333703, 0.3333333333333333703, 0.3333333333333333703, 0.3333333333333333703, 0.3333333333333333703, 0.3333333333333333703, 0.3333333333333333703, 0.3333333333333333703, 0.3333333333333333703, 0.3333333333333333703, 0.3333333333333333703, 0.3333333333333333703, 0.3333333333333333703, 0.3333333333333333703, 0.3333333333333333703, 0.3333333333333333703, 0.3333333333333333703, 0.3333333333333333703, 0.3333333333333333703, 0.3333333333333333703, 0.3333333333333333703, 0.3333333333333333703, 0.3333333333333333703, 0.3333333333333333703, 0.3333333333333333703, 0.3333333333333333703, 0.3333333333333333703, 0.3333333333333333703, 0.3333333333333333703, 0.3333333333333333703, 0.3333333333333333703, 0.3333333333333333703, 0.3333333333333333703, 0.3333333333333333703, 0.3333333333333333703, 0.3333333333333333703, 0.3333333333333333703, 0.3333333333333333703, 0.3333333333333333703, 0.3333333333333333703, 0.3333333333333333703, 0.3333333333333333703, 0.3333333333333333703, 0.3333333333333333703, 0.3333333333333333703, 0.3333333333333333703, 0.3333333333333333703, 0.3333333333333333703, 0.3333333333333333703, 0.3333333333333333703, 0.3333333333333333703, 0.3333333333333333703, 0.3333333333333333703, 0.3333333333333333703, 0.3333333333333333703, 0.3333333333333333703, 0.3333333333333333703, 0.3333333333333333703),
 ( 1.000000000000000000, 1.000000000000000000, 1.000000000000000000, 1.000000000000000000, 1.000000000000000000, 1.000000000000000000, 1.000000000000000000, 1.000000000000000000, 1.000000000000000000, 1.000000000000000000, 1.000000000000000000, 1.000000000000000000, 1.000000000000000000, 1.000000000000000000, 1.000000000000000000, 1.000000000000000000, 1.000000000000000000, 1.000000000000000000, 1.000000000000000000, 1.000000000000000000, 1.000000000000000000, 1.000000000000000000, 1.000000000000000000, 1.000000000000000000, 1.000000000000000000, 1.000000000000000000, 1.000000000000000000, 1.000000000000000000, 1.000000000000000000, 1.000000000000000000, 1.000000000000000000, 1.000000000000000000, 1.000000000000000000, 1.000000000000000000, 1.000000000000000000, 1.000000000000000000, 1.000000000000000000, 1.000000000000000000, 1.000000000000000000, 1.000000000000000000, 1.000000000000000000, 1.000000000000000000, 1.000000000000000000, 1.000000000000000000, 1.000000000000000000, 1.000000000000000000, 1.000000000000000000, 1.000000000000000000, 1.000000000000000000, 1.000000000000000000, 1.000000000000000000, 1.000000000000000000, 1.000000000000000000, 1.000000000000000000, 1.000000000000000000, 1.000000000000000000, 1.000000000000000000, 1.000000000000000000, 1.000000000000000000, 1.000000000000000000, 1.000000000000000000, 1.000000000000000000, 1.000000000000000000, 1.000000000000000000, 1.000000000000000000, 1.000000000000000000, 1.000000000000000000, 1.000000000000000000, 1.000000000000000000, 1.000000000000000000, 1.000000000000000000, 1.000000000000000000, 1.000000000000000000, 1.000000000000000000, 1.000000000000000000, 1.000000000000000000, 1.000000000000000000, 1.000000000000000000, 1.000000000000000000, 1.000000000000000000, 1.000000000000000000, 1.000000000000000000, 1.000000000000000000, 1.000000000000000000, 1.000000000000000000, 1.000000000000000000, 1.000000000000000000, 1.000000000000000000, 1.000000000000000000, 1.000000000000000000, 1.000000000000000000, 1.000000000000000000, 1.000000000000000000, 1.000000000000000000, 1.000000000000000000, 1.000000000000000000, 1.000000000000000000, 1.000000000000000000, 1.000000000000000000, 1.000000000000000000, 1.000000000000000000, 1.000000000000000000, 1.000000000000000000, 1.000000000000000000, 1.000000000000000000, 1.000000000000000000, 1.000000000000000000, 1.000000000000000000, 1.000000000000000000, 1.000000000000000000, 1.000000000000000000, 1.000000000000000000, 1.000000000000000000, 1.000000000000000000, 1.000000000000000000, 1.000000000000000000, 1.000000000000000000, 1.000000000000000000, 1.000000000000000000, 1.000000000000000000, 1.000000000000000000, 1.000000000000000000, 1.000000000000000000, 1.000000000000000000, 1.000000000000000000, 1.000000000000000000, 1.000000000000000000, 1.000000000000000000, 1.000000000000000000, 1.000000000000000000, 1.000000000000000000, 1.000000000000000000, 1.000000000000000000, 1.000000000000000000, 1.000000000000000000, 1.000000000000000000, 1.000000000000000000, 1.000000000000000000, 1.000000000000000000, 1.000000000000000000, 1.000000000000000000, 1.000000000000000000, 1.000000000000000000, 1.000000000000000000, 1.000000000000000000, 1.000000000000000000, 1.000000000000000000, 1.000000000000000000, 1.000000000000000000, 1.000000000000000000, 1.000000000000000000, 1.000000000000000000, 1.000000000000000000, 1.000000000000000000, 1.000000000000000000, 1.000000000000000000, 1.000000000000000000, 1.000000000000000000, 1.000000000000000000, 1.000000000000000000, 1.000000000000000000, 1.000000000000000000, 1.000000000000000000, 1.000000000000000000, 1.000000000000000000, 1.000000000000000000, 1.000000000000000000, 1.000000000000000000, 1.000000000000000000, 1.000000000000000000, 1.000000000000000000, 1.000000000000000000, 1.000000000000000000, 1.000000000000000000, 1.000000000000000000, 1.000000000000000000, 1.000000000000000000, 1.000000000000000000, 1.000000000000000000, 1.000000000000000000, 1.000000000000000000, 1.000000000000000000, 1.000000000000000000, 1.000000000000000000, 1.000000000000000000, 1.000000000000000000, 1.000000000000000000, 1.000000000000000000, 1.000000000000000000, 1.000000000000000000, 1.000000000000000000, 1.000000000000000000, 1.000000000000000000, 1.000000000000000000, 1.000000000000000000, 1.000000000000000000, 1.000000000000000000, 1.000000000000000000, 1.000000000000000000, 1.000000000000000000, 1.000000000000000000, 1.000000000000000000, 1.000000000000000000, 1.000000000000000000, 1.000000000000000000, 1.000000000000000000, 1.000000000000000000, 1.000000000000000000, 1.000000000000000000, 1.000000000000000000, 1.000000000000000000, 1.000000000000000000, 1.000000000000000000, 1.000000000000000000, 1.000000000000000000, 1.000000000000000000, 1.000000000000000000, 1.000000000000000000, 1.000000000000000000, 1.000000000000000000, 1.000000000000000000, 1.000000000000000000, 1.000000000000000000, 1.000000000000000000, 1.000000000000000000, 1.000000000000000000, 1.000000000000000000, 1.000000000000000000, 1.000000000000000000, 1.000000000000000000, 1.000000000000000000, 1.000000000000000000, 1.000000000000000000, 1.000000000000000000, 1.000000000000000000, 1.000000000000000000, 1.000000000000000000, 1.000000000000000000, 1.000000000000000000, 1.000000000000000000, 1.000000000000000000, 1.000000000000000000, 1.000000000000000000, 1.000000000000000000, 1.000000000000000000, 1.000000000000000000, 1.000000000000000000, 1.000000000000000000, 1.000000000000000000, 1.000000000000000000, 1.000000000000000000, 1.000000000000000000, 1.000000000000000000, 1.000000000000000000, 1.000000000000000000, 1.000000000000000000, 1.000000000000000000, 1.000000000000000000, 1.000000000000000000, 1.000000000000000000, 1.000000000000000000, 1.000000000000000000, 1.000000000000000000, 1.000000000000000000, 1.000000000000000000, 1.000000000000000000, 1.000000000000000000, 1.000000000000000000, 1.000000000000000000, 1.000000000000000000, 1.000000000000000000, 1.000000000000000000, 1.000000000000000000, 1.000000000000000000, 1.000000000000000000, 1.000000000000000000, 1.000000000000000000, 1.000000000000000000, 1.000000000000000000, 1.000000000000000000, 1.000000000000000000, 1.000000000000000000, 1.000000000000000000, 1.000000000000000000, 1.000000000000000000, 1.000000000000000000, 1.000000000000000000, 1.000000000000000000, 1.000000000000000000, 1.000000000000000000, 1.000000000000000000, 1.000000000000000000, 1.000000000000000000, 1.000000000000000000, 1.000000000000000000, 1.000000000000000000, 1.000000000000000000, 1.000000000000000000, 1.000000000000000000, 1.000000000000000000, 1.000000000000000000, 1.000000000000000000, 1.000000000000000000, 1.000000000000000000, 1.000000000000000000, 1.000000000000000000, 1.000000000000000000, 1.000000000000000000, 1.000000000000000000, 1.000000000000000000, 1.000000000000000000, 1.000000000000000000, 1.000000000000000000, 1.000000000000000000, 1.000000000000000000, 1.000000000000000000, 1.000000000000000000, 1.000000000000000000, 1.000000000000000000, 1.000000000000000000, 1.000000000000000000, 1.000000000000000000, 1.000000000000000000, 1.000000000000000000, 1.000000000000000000, 1.000000000000000000, 1.000000000000000000, 1.000000000000000000, 1.000000000000000000, 1.000000000000000000, 1.000000000000000000, 1.000000000000000000, 1.000000000000000000, 1.000000000000000000, 1.000000000000000000, 1.000000000000000000),
 ( 0.3333333333333333703, 0.3333333333333333703, 0.3333333333333333703, 0.3333333333333333703, 0.3333333333333333703, 0.3333333333333333703, 0.3333333333333333703, 0.3333333333333333703, 0.3333333333333333703, 0.3333333333333333703, 0.3333333333333333703, 0.3333333333333333703, 0.3333333333333333703, 0.3333333333333333703, 0.3333333333333333703, 0.3333333333333333703, 0.3333333333333333703, 0.3333333333333333703, 0.3333333333333333703, 0.3333333333333333703, 0.3333333333333333703, 0.3333333333333333703, 0.3333333333333333703, 0.3333333333333333703, 0.3333333333333333703, 0.3333333333333333703, 0.3333333333333333703, 0.3333333333333333703, 0.3333333333333333703, 0.3333333333333333703, 0.3333333333333333703, 0.3333333333333333703, 0.3333333333333333703, 0.3333333333333333703, 0.3333333333333333703, 0.3333333333333333703, 0.3333333333333333703, 0.3333333333333333703, 0.3333333333333333703, 0.3333333333333333703, 0.3333333333333333703, 0.3333333333333333703, 0.3333333333333333703, 0.3333333333333333703, 0.3333333333333333703, 0.3333333333333333703, 0.3333333333333333703, 0.3333333333333333703, 0.3333333333333333703, 0.3333333333333333703, 0.3333333333333333703, 0.3333333333333333703, 0.3333333333333333703, 0.3333333333333333703, 0.3333333333333333703, 0.3333333333333333703, 0.3333333333333333703, 0.3333333333333333703, 0.3333333333333333703, 0.3333333333333333703, 0.3333333333333333703, 0.3333333333333333703, 0.3333333333333333703, 0.3333333333333333703, 0.3333333333333333703, 0.3333333333333333703, 0.3333333333333333703, 0.3333333333333333703, 0.3333333333333333703, 0.3333333333333333703, 0.3333333333333333703, 0.3333333333333333703, 0.3333333333333333703, 0.3333333333333333703, 0.3333333333333333703, 0.3333333333333333703, 0.3333333333333333703, 0.3333333333333333703, 0.3333333333333333703, 0.3333333333333333703, 0.3333333333333333703, 0.3333333333333333703, 0.3333333333333333703, 0.3333333333333333703, 0.3333333333333333703, 0.3333333333333333703, 0.3333333333333333703, 0.3333333333333333703, 0.3333333333333333703, 0.3333333333333333703, 0.3333333333333333703, 0.3333333333333333703, 0.3333333333333333703, 0.3333333333333333703, 0.3333333333333333703, 0.3333333333333333703, 0.3333333333333333703, 0.3333333333333333703, 0.3333333333333333703, 0.3333333333333333703, 0.3333333333333333703, 0.3333333333333333703, 0.3333333333333333703, 0.3333333333333333703, 0.3333333333333333703, 0.3333333333333333703, 0.3333333333333333703, 0.3333333333333333703, 0.3333333333333333703, 0.3333333333333333703, 0.3333333333333333703, 0.3333333333333333703, 0.3333333333333333703, 0.3333333333333333703, 0.3333333333333333703, 0.3333333333333333703, 0.3333333333333333703, 0.3333333333333333703, 0.3333333333333333703, 0.3333333333333333703, 0.3333333333333333703, 0.3333333333333333703, 0.3333333333333333703, 0.3333333333333333703, 0.3333333333333333703, 0.3333333333333333703, 0.3333333333333333703, 0.3333333333333333703, 0.3333333333333333703, 0.3333333333333333703, 0.3333333333333333703, 0.3333333333333333703, 0.3333333333333333703, 0.3333333333333333703, 0.3333333333333333703, 0.3333333333333333703, 0.3333333333333333703, 0.3333333333333333703, 0.3333333333333333703, 0.3333333333333333703, 0.3333333333333333703, 0.3333333333333333703, 0.3333333333333333703, 0.3333333333333333703, 0.3333333333333333703, 0.3333333333333333703, 0.3333333333333333703, 0.3333333333333333703, 0.3333333333333333703, 0.3333333333333333703, 0.3333333333333333703, 0.3333333333333333703, 0.3333333333333333703, 0.3333333333333333703, 0.3333333333333333703, 0.3333333333333333703, 0.3333333333333333703, 0.3333333333333333703, 0.3333333333333333703, 0.3333333333333333703, 0.3333333333333333703, 0.3333333333333333703, 0.3333333333333333703, 0.3333333333333333703, 0.3333333333333333703, 0.3333333333333333703, 0.3333333333333333703, 0.3333333333333333703, 0.3333333333333333703, 0.3333333333333333703, 0.3333333333333333703, 0.3333333333333333703, 0.3333333333333333703, 0.3333333333333333703, 0.3333333333333333703, 0.3333333333333333703, 0.3333333333333333703, 0.3333333333333333703, 0.3333333333333333703, 0.3333333333333333703, 0.3333333333333333703, 0.3333333333333333703, 0.3333333333333333703, 0.3333333333333333703, 0.3333333333333333703, 0.3333333333333333703, 0.3333333333333333703, 0.3333333333333333703, 0.3333333333333333703, 0.3333333333333333703, 0.3333333333333333703, 0.3333333333333333703, 0.3333333333333333703, 0.3333333333333333703, 0.3333333333333333703, 0.3333333333333333703, 0.3333333333333333703, 0.3333333333333333703, 0.3333333333333333703, 0.3333333333333333703, 0.3333333333333333703, 0.3333333333333333703, 0.3333333333333333703, 0.3333333333333333703, 0.3333333333333333703, 0.3333333333333333703, 0.3333333333333333703, 0.3333333333333333703, 0.3333333333333333703, 0.3333333333333333703, 0.3333333333333333703, 0.3333333333333333703, 0.3333333333333333703, 0.3333333333333333703, 0.3333333333333333703, 0.3333333333333333703, 0.3333333333333333703, 0.3333333333333333703, 0.3333333333333333703, 0.3333333333333333703, 0.3333333333333333703, 0.3333333333333333703, 0.3333333333333333703, 0.3333333333333333703, 0.3333333333333333703, 0.3333333333333333703, 0.3333333333333333703, 0.3333333333333333703, 0.3333333333333333703, 0.3333333333333333703, 0.3333333333333333703, 0.3333333333333333703, 0.3333333333333333703, 0.3333333333333333703, 0.3333333333333333703, 0.3333333333333333703, 0.3333333333333333703, 0.3333333333333333703, 0.3333333333333333703, 0.3333333333333333703, 0.3333333333333333703, 0.3333333333333333703, 0.3333333333333333703, 0.3333333333333333703, 0.3333333333333333703, 0.3333333333333333703, 0.3333333333333333703, 0.3333333333333333703, 0.3333333333333333703, 0.3333333333333333703, 0.3333333333333333703, 0.3333333333333333703, 0.3333333333333333703, 0.3333333333333333703, 0.3333333333333333703, 0.3333333333333333703, 0.3333333333333333703, 0.3333333333333333703, 0.3333333333333333703, 0.3333333333333333703, 0.3333333333333333703, 0.3333333333333333703, 0.3333333333333333703, 0.3333333333333333703, 0.3333333333333333703, 0.3333333333333333703, 0.3333333333333333703, 0.3333333333333333703, 0.3333333333333333703, 0.3333333333333333703, 0.3333333333333333703, 0.3333333333333333703, 0.3333333333333333703, 0.3333333333333333703, 0.3333333333333333703, 0.3333333333333333703, 0.3333333333333333703, 0.3333333333333333703, 0.3333333333333333703, 0.3333333333333333703, 0.3333333333333333703, 0.3333333333333333703, 0.3333333333333333703, 0.3333333333333333703, 0.3333333333333333703, 0.3333333333333333703, 0.3333333333333333703, 0.3333333333333333703, 0.3333333333333333703, 0.3333333333333333703, 0.3333333333333333703, 0.3333333333333333703, 0.3333333333333333703, 0.3333333333333333703, 0.3333333333333333703, 0.3333333333333333703, 0.3333333333333333703, 0.3333333333333333703, 0.3333333333333333703, 0.3333333333333333703, 0.3333333333333333703, 0.3333333333333333703, 0.3333333333333333703, 0.3333333333333333703, 0.3333333333333333703, 0.3333333333333333703, 0.3333333333333333703, 0.3333333333333333703, 0.3333333333333333703, 0.3333333333333333703, 0.3333333333333333703, 0.3333333333333333703, 0.3333333333333333703, 0.3333333333333333703, 0.3333333333333333703, 0.3333333333333333703, 0.3333333333333333703, 0.3333333333333333703, 0.3333333333333333703, 0.3333333333333333703, 0.3333333333333333703, 0.3333333333333333703, 0.3333333333333333703, 0.3333333333333333703, 0.3333333333333333703, 0.3333333333333333703, 0.3333333333333333703, 0.3333333333333333703, 0.3333333333333333703, 0.3333333333333333703, 0.3333333333333333703, 0.3333333333333333703, 0.3333333333333333703, 0.3333333333333333703, 0.3333333333333333703, 0.3333333333333333703),
 ( 0.3333333333333333703, 0.3333333333333333703, 0.3333333333333333703, 0.3333333333333333703, 0.3333333333333333703, 0.3333333333333333703, 0.3333333333333333703, 0.3333333333333333703, 0.3333333333333333703, 0.3333333333333333703, 0.3333333333333333703, 0.3333333333333333703, 0.3333333333333333703, 0.3333333333333333703, 0.3333333333333333703, 0.3333333333333333703, 0.3333333333333333703, 0.3333333333333333703, 0.3333333333333333703, 0.3333333333333333703, 0.3333333333333333703, 0.3333333333333333703, 0.3333333333333333703, 0.3333333333333333703, 0.3333333333333333703, 0.3333333333333333703, 0.3333333333333333703, 0.3333333333333333703, 0.3333333333333333703, 0.3333333333333333703, 0.3333333333333333703, 0.3333333333333333703, 0.3333333333333333703, 0.3333333333333333703, 0.3333333333333333703, 0.3333333333333333703, 0.3333333333333333703, 0.3333333333333333703, 0.3333333333333333703, 0.3333333333333333703, 0.3333333333333333703, 0.3333333333333333703, 0.3333333333333333703, 0.3333333333333333703, 0.3333333333333333703, 0.3333333333333333703, 0.3333333333333333703, 0.3333333333333333703, 0.3333333333333333703, 0.3333333333333333703, 0.3333333333333333703, 0.3333333333333333703, 0.3333333333333333703, 0.3333333333333333703, 0.3333333333333333703, 0.3333333333333333703, 0.3333333333333333703, 0.3333333333333333703, 0.3333333333333333703, 0.3333333333333333703, 0.3333333333333333703, 0.3333333333333333703, 0.3333333333333333703, 0.3333333333333333703, 0.3333333333333333703, 0.3333333333333333703, 0.3333333333333333703, 0.3333333333333333703, 0.3333333333333333703, 0.3333333333333333703, 0.3333333333333333703, 0.3333333333333333703, 0.3333333333333333703, 0.3333333333333333703, 0.3333333333333333703, 0.3333333333333333703, 0.3333333333333333703, 0.3333333333333333703, 0.3333333333333333703, 0.3333333333333333703, 0.3333333333333333703, 0.3333333333333333703, 0.3333333333333333703, 0.3333333333333333703, 0.3333333333333333703, 0.3333333333333333703, 0.3333333333333333703, 0.3333333333333333703, 0.3333333333333333703, 0.3333333333333333703, 0.3333333333333333703, 0.3333333333333333703, 0.3333333333333333703, 0.3333333333333333703, 0.3333333333333333703, 0.3333333333333333703, 0.3333333333333333703, 0.3333333333333333703, 0.3333333333333333703, 0.3333333333333333703, 0.3333333333333333703, 0.3333333333333333703, 0.3333333333333333703, 0.3333333333333333703, 0.3333333333333333703, 0.3333333333333333703, 0.3333333333333333703, 0.3333333333333333703, 0.3333333333333333703, 0.3333333333333333703, 0.3333333333333333703, 0.3333333333333333703, 0.3333333333333333703, 0.3333333333333333703, 0.3333333333333333703, 0.3333333333333333703, 0.3333333333333333703, 0.3333333333333333703, 0.3333333333333333703, 0.3333333333333333703, 0.3333333333333333703, 0.3333333333333333703, 0.3333333333333333703, 0.3333333333333333703, 0.3333333333333333703, 0.3333333333333333703, 0.3333333333333333703, 0.3333333333333333703, 0.3333333333333333703, 0.3333333333333333703, 0.3333333333333333703, 0.3333333333333333703, 0.3333333333333333703, 0.3333333333333333703, 0.3333333333333333703, 0.3333333333333333703, 0.3333333333333333703, 0.3333333333333333703, 0.3333333333333333703, 0.3333333333333333703, 0.3333333333333333703, 0.3333333333333333703, 0.3333333333333333703, 0.3333333333333333703, 0.3333333333333333703, 0.3333333333333333703, 0.3333333333333333703, 0.3333333333333333703, 0.3333333333333333703, 0.3333333333333333703, 0.3333333333333333703, 0.3333333333333333703, 0.3333333333333333703, 0.3333333333333333703, 0.3333333333333333703, 0.3333333333333333703, 0.3333333333333333703, 0.3333333333333333703, 0.3333333333333333703, 0.3333333333333333703, 0.3333333333333333703, 0.3333333333333333703, 0.3333333333333333703, 0.3333333333333333703, 0.3333333333333333703, 0.3333333333333333703, 0.3333333333333333703, 0.3333333333333333703, 0.3333333333333333703, 0.3333333333333333703, 0.3333333333333333703, 0.3333333333333333703, 0.3333333333333333703, 0.3333333333333333703, 0.3333333333333333703, 0.3333333333333333703, 0.3333333333333333703, 0.3333333333333333703, 0.3333333333333333703, 0.3333333333333333703, 0.3333333333333333703, 0.3333333333333333703, 0.3333333333333333703, 0.3333333333333333703, 0.3333333333333333703, 0.3333333333333333703, 0.3333333333333333703, 0.3333333333333333703, 0.3333333333333333703, 0.3333333333333333703, 0.3333333333333333703, 0.3333333333333333703, 0.3333333333333333703, 0.3333333333333333703, 0.3333333333333333703, 0.3333333333333333703, 0.3333333333333333703, 0.3333333333333333703, 0.3333333333333333703, 0.3333333333333333703, 0.3333333333333333703, 0.3333333333333333703, 0.3333333333333333703, 0.3333333333333333703, 0.3333333333333333703, 0.3333333333333333703, 0.3333333333333333703, 0.3333333333333333703, 0.3333333333333333703, 0.3333333333333333703, 0.3333333333333333703, 0.3333333333333333703, 0.3333333333333333703, 0.3333333333333333703, 0.3333333333333333703, 0.3333333333333333703, 0.3333333333333333703, 0.3333333333333333703, 0.3333333333333333703, 0.3333333333333333703, 0.3333333333333333703, 0.3333333333333333703, 0.3333333333333333703, 0.3333333333333333703, 0.3333333333333333703, 0.3333333333333333703, 0.3333333333333333703, 0.3333333333333333703, 0.3333333333333333703, 0.3333333333333333703, 0.3333333333333333703, 0.3333333333333333703, 0.3333333333333333703, 0.3333333333333333703, 0.3333333333333333703, 0.3333333333333333703, 0.3333333333333333703, 0.3333333333333333703, 0.3333333333333333703, 0.3333333333333333703, 0.3333333333333333703, 0.3333333333333333703, 0.3333333333333333703, 0.3333333333333333703, 0.3333333333333333703, 0.3333333333333333703, 0.3333333333333333703, 0.3333333333333333703, 0.3333333333333333703, 0.3333333333333333703, 0.3333333333333333703, 0.3333333333333333703, 0.3333333333333333703, 0.3333333333333333703, 0.3333333333333333703, 0.3333333333333333703, 0.3333333333333333703, 0.3333333333333333703, 0.3333333333333333703, 0.3333333333333333703, 0.3333333333333333703, 0.3333333333333333703, 0.3333333333333333703, 0.3333333333333333703, 0.3333333333333333703, 0.3333333333333333703, 0.3333333333333333703, 0.3333333333333333703, 0.3333333333333333703, 0.3333333333333333703, 0.3333333333333333703, 0.3333333333333333703, 0.3333333333333333703, 0.3333333333333333703, 0.3333333333333333703, 0.3333333333333333703, 0.3333333333333333703, 0.3333333333333333703, 0.3333333333333333703, 0.3333333333333333703, 0.3333333333333333703, 0.3333333333333333703, 0.3333333333333333703, 0.3333333333333333703, 0.3333333333333333703, 0.3333333333333333703, 0.3333333333333333703, 0.3333333333333333703, 0.3333333333333333703, 0.3333333333333333703, 0.3333333333333333703, 0.3333333333333333703, 0.3333333333333333703, 0.3333333333333333703, 0.3333333333333333703, 0.3333333333333333703, 0.3333333333333333703, 0.3333333333333333703, 0.3333333333333333703, 0.3333333333333333703, 0.3333333333333333703, 0.3333333333333333703, 0.3333333333333333703, 0.3333333333333333703, 0.3333333333333333703, 0.3333333333333333703, 0.3333333333333333703, 0.3333333333333333703, 0.3333333333333333703, 0.3333333333333333703, 0.3333333333333333703, 0.3333333333333333703, 0.3333333333333333703, 0.3333333333333333703, 0.3333333333333333703, 0.3333333333333333703, 0.3333333333333333703, 0.3333333333333333703, 0.3333333333333333703, 0.3333333333333333703, 0.3333333333333333703, 0.3333333333333333703, 0.3333333333333333703, 0.3333333333333333703, 0.3333333333333333703, 0.3333333333333333703, 0.3333333333333333703, 0.3333333333333333703, 0.3333333333333333703, 0.3333333333333333703, 0.3333333333333333703, 0.3333333333333333703, 0.3333333333333333703, 0.3333333333333333703, 0.3333333333333333703, 0.3333333333333333703),
 ( 1.000000000000000000, 1.000000000000000000, 1.000000000000000000, 1.000000000000000000, 1.000000000000000000, 1.000000000000000000, 1.000000000000000000, 1.000000000000000000, 1.000000000000000000, 1.000000000000000000, 1.000000000000000000, 1.000000000000000000, 1.000000000000000000, 1.000000000000000000, 1.000000000000000000, 1.000000000000000000, 1.000000000000000000, 1.000000000000000000, 1.000000000000000000, 1.000000000000000000, 1.000000000000000000, 1.000000000000000000, 1.000000000000000000, 1.000000000000000000, 1.000000000000000000, 1.000000000000000000, 1.000000000000000000, 1.000000000000000000, 1.000000000000000000, 1.000000000000000000, 1.000000000000000000, 1.000000000000000000, 1.000000000000000000, 1.000000000000000000, 1.000000000000000000, 1.000000000000000000, 1.000000000000000000, 1.000000000000000000, 1.000000000000000000, 1.000000000000000000, 1.000000000000000000, 1.000000000000000000, 1.000000000000000000, 1.000000000000000000, 1.000000000000000000, 1.000000000000000000, 1.000000000000000000, 1.000000000000000000, 1.000000000000000000, 1.000000000000000000, 1.000000000000000000, 1.000000000000000000, 1.000000000000000000, 1.000000000000000000, 1.000000000000000000, 1.000000000000000000, 1.000000000000000000, 1.000000000000000000, 1.000000000000000000, 1.000000000000000000, 1.000000000000000000, 1.000000000000000000, 1.000000000000000000, 1.000000000000000000, 1.000000000000000000, 1.000000000000000000, 1.000000000000000000, 1.000000000000000000, 1.000000000000000000, 1.000000000000000000, 1.000000000000000000, 1.000000000000000000, 1.000000000000000000, 1.000000000000000000, 1.000000000000000000, 1.000000000000000000, 1.000000000000000000, 1.000000000000000000, 1.000000000000000000, 1.000000000000000000, 1.000000000000000000, 1.000000000000000000, 1.000000000000000000, 1.000000000000000000, 1.000000000000000000, 1.000000000000000000, 1.000000000000000000, 1.000000000000000000, 1.000000000000000000, 1.000000000000000000, 1.000000000000000000, 1.000000000000000000, 1.000000000000000000, 1.000000000000000000, 1.000000000000000000, 1.000000000000000000, 1.000000000000000000, 1.000000000000000000, 1.000000000000000000, 1.000000000000000000, 1.000000000000000000, 1.000000000000000000, 1.000000000000000000, 1.000000000000000000, 1.000000000000000000, 1.000000000000000000, 1.000000000000000000, 1.000000000000000000, 1.000000000000000000, 1.000000000000000000, 1.000000000000000000, 1.000000000000000000, 1.000000000000000000, 1.000000000000000000, 1.000000000000000000, 1.000000000000000000, 1.000000000000000000, 1.000000000000000000, 1.000000000000000000, 1.000000000000000000, 1.000000000000000000, 1.000000000000000000, 1.000000000000000000, 1.000000000000000000, 1.000000000000000000, 1.000000000000000000, 1.000000000000000000, 1.000000000000000000, 1.000000000000000000, 1.000000000000000000, 1.000000000000000000, 1.000000000000000000, 1.000000000000000000, 1.000000000000000000, 1.000000000000000000, 1.000000000000000000, 1.000000000000000000, 1.000000000000000000, 1.000000000000000000, 1.000000000000000000, 1.000000000000000000, 1.000000000000000000, 1.000000000000000000, 1.000000000000000000, 1.000000000000000000, 1.000000000000000000, 1.000000000000000000, 1.000000000000000000, 1.000000000000000000, 1.000000000000000000, 1.000000000000000000, 1.000000000000000000, 1.000000000000000000, 1.000000000000000000, 1.000000000000000000, 1.000000000000000000, 1.000000000000000000, 1.000000000000000000, 1.000000000000000000, 1.000000000000000000, 1.000000000000000000, 1.000000000000000000, 1.000000000000000000, 1.000000000000000000, 1.000000000000000000, 1.000000000000000000, 1.000000000000000000, 1.000000000000000000, 1.000000000000000000, 1.000000000000000000, 1.000000000000000000, 1.000000000000000000, 1.000000000000000000, 1.000000000000000000, 1.000000000000000000, 1.000000000000000000, 1.000000000000000000, 1.000000000000000000, 1.000000000000000000, 1.000000000000000000, 1.000000000000000000, 1.000000000000000000, 1.000000000000000000, 1.000000000000000000, 1.000000000000000000, 1.000000000000000000, 1.000000000000000000, 1.000000000000000000, 1.000000000000000000, 1.000000000000000000, 1.000000000000000000, 1.000000000000000000, 1.000000000000000000, 1.000000000000000000, 1.000000000000000000, 1.000000000000000000, 1.000000000000000000, 1.000000000000000000, 1.000000000000000000, 1.000000000000000000, 1.000000000000000000, 1.000000000000000000, 1.000000000000000000, 1.000000000000000000, 1.000000000000000000, 1.000000000000000000, 1.000000000000000000, 1.000000000000000000, 1.000000000000000000, 1.000000000000000000, 1.000000000000000000, 1.000000000000000000, 1.000000000000000000, 1.000000000000000000, 1.000000000000000000, 1.000000000000000000, 1.000000000000000000, 1.000000000000000000, 1.000000000000000000, 1.000000000000000000, 1.000000000000000000, 1.000000000000000000, 1.000000000000000000, 1.000000000000000000, 1.000000000000000000, 1.000000000000000000, 1.000000000000000000, 1.000000000000000000, 1.000000000000000000, 1.000000000000000000, 1.000000000000000000, 1.000000000000000000, 1.000000000000000000, 1.000000000000000000, 1.000000000000000000, 1.000000000000000000, 1.000000000000000000, 1.000000000000000000, 1.000000000000000000, 1.000000000000000000, 1.000000000000000000, 1.000000000000000000, 1.000000000000000000, 1.000000000000000000, 1.000000000000000000, 1.000000000000000000, 1.000000000000000000, 1.000000000000000000, 1.000000000000000000, 1.000000000000000000, 1.000000000000000000, 1.000000000000000000, 1.000000000000000000, 1.000000000000000000, 1.000000000000000000, 1.000000000000000000, 1.000000000000000000, 1.000000000000000000, 1.000000000000000000, 1.000000000000000000, 1.000000000000000000, 1.000000000000000000, 1.000000000000000000, 1.000000000000000000, 1.000000000000000000, 1.000000000000000000, 1.000000000000000000, 1.000000000000000000, 1.000000000000000000, 1.000000000000000000, 1.000000000000000000, 1.000000000000000000, 1.000000000000000000, 1.000000000000000000, 1.000000000000000000, 1.000000000000000000, 1.000000000000000000, 1.000000000000000000, 1.000000000000000000, 1.000000000000000000, 1.000000000000000000, 1.000000000000000000, 1.000000000000000000, 1.000000000000000000, 1.000000000000000000, 1.000000000000000000, 1.000000000000000000, 1.000000000000000000, 1.000000000000000000, 1.000000000000000000, 1.000000000000000000, 1.000000000000000000, 1.000000000000000000, 1.000000000000000000, 1.000000000000000000, 1.000000000000000000, 1.000000000000000000, 1.000000000000000000, 1.000000000000000000, 1.000000000000000000, 1.000000000000000000, 1.000000000000000000, 1.000000000000000000, 1.000000000000000000, 1.000000000000000000, 1.000000000000000000, 1.000000000000000000, 1.000000000000000000, 1.000000000000000000, 1.000000000000000000, 1.000000000000000000, 1.000000000000000000, 1.000000000000000000, 1.000000000000000000, 1.000000000000000000, 1.000000000000000000, 1.000000000000000000, 1.000000000000000000, 1.000000000000000000, 1.000000000000000000, 1.000000000000000000, 1.000000000000000000, 1.000000000000000000, 1.000000000000000000, 1.000000000000000000, 1.000000000000000000, 1.000000000000000000, 1.000000000000000000, 1.000000000000000000, 1.000000000000000000, 1.000000000000000000, 1.000000000000000000, 1.000000000000000000, 1.000000000000000000, 1.000000000000000000, 1.000000000000000000) ) ) 
 REPRESENTATION_ITEM ( '' )  SURFACE ( )  );
#5403 = CARTESIAN_POINT ( 'NONE',  ( -31.58308234758948174, -0.5371106682196264970, -221.7519263543700845 ) ) ;
#5404 = ORIENTED_EDGE ( 'NONE', *, *, #21485, .F. ) ;
#5405 = CARTESIAN_POINT ( 'NONE',  ( -13.68337831708448782, -3.656824064325736590, -221.3737413816871538 ) ) ;
#5406 = ADVANCED_FACE ( 'NONE', ( #8529 ), #13700, .T. ) ;
#5407 = CARTESIAN_POINT ( 'NONE',  ( -11.19105919052231179, 21.17456633634251872, -216.2128528132037957 ) ) ;
#5408 = CARTESIAN_POINT ( 'NONE',  ( -7.349743644505656093, -15.31718010764164539, -232.4470764718129772 ) ) ;
#5409 = CARTESIAN_POINT ( 'NONE',  ( 4.340445191644851874, 29.86837761166362881, -227.4879512554873315 ) ) ;
#5410 = CARTESIAN_POINT ( 'NONE',  ( 4.449544252370068342, -12.87211356511098082, -219.5022864574935113 ) ) ;
#5411 = CARTESIAN_POINT ( 'NONE',  ( -26.22594988380878789, -0.1068133454905619700, -219.1167922977186322 ) ) ;
#5412 = ADVANCED_FACE ( 'NONE', ( #6485 ), #13009, .T. ) ;
#5413 = CARTESIAN_POINT ( 'NONE',  ( -26.02492405343843984, 6.940268742526972900, -218.8798307745116460 ) ) ;
#5414 = CYLINDRICAL_SURFACE ( 'NONE', #10653, 10.00000000000000000 ) ;
#5415 = CARTESIAN_POINT ( 'NONE',  ( -2.693916085894628942, 18.86613858709357672, -230.4911878356387263 ) ) ;
#5416 = CARTESIAN_POINT ( 'NONE',  ( -21.43408368508570305, 3.680162304907783621, -233.1134812316964542 ) ) ;
#5417 = CARTESIAN_POINT ( 'NONE',  ( 14.22574309452842733, 4.476723532073429546, -225.5862451792618231 ) ) ;
#5418 = CARTESIAN_POINT ( 'NONE',  ( 26.39436175479395885, 14.32821500273865034, -221.6819523832376149 ) ) ;
#5419 = CARTESIAN_POINT ( 'NONE',  ( 4.210909054564462295, -12.48022235161367988, -220.2789660014272215 ) ) ;
#5420 = EDGE_CURVE ( 'NONE', #3391, #9522, #4908, .T. ) ;
#5421 = CARTESIAN_POINT ( 'NONE',  ( 11.38520239593705163, 18.87760105923376486, -235.3435298574111130 ) ) ;
#5422 = CARTESIAN_POINT ( 'NONE',  ( 0.000000000000000000, -23.00000000000000000, 75.00000000000000000 ) ) ;
#5423 = CARTESIAN_POINT ( 'NONE',  ( -1.366762408920091598, -18.58806247050231875, -233.7525452272278699 ) ) ;
#5424 = CARTESIAN_POINT ( 'NONE',  ( -4.073886805163430935, 14.35067061637828623, -226.4733297826468572 ) ) ;
#5425 = CARTESIAN_POINT ( 'NONE',  ( 7.018811797190238622, 13.93862807232938472, -230.2855929063610176 ) ) ;
#5426 = CARTESIAN_POINT ( 'NONE',  ( -20.85586116824185510, -1.996934699305910499, -232.3804859832740135 ) ) ;
#5427 = CARTESIAN_POINT ( 'NONE',  ( -15.47996233766743934, 8.203483081506188768, -221.0931279926996353 ) ) ;
#5428 = CARTESIAN_POINT ( 'NONE',  ( -0.6224962293416278492, 14.12372964796689701, -218.2103911528446645 ) ) ;
#5429 = CARTESIAN_POINT ( 'NONE',  ( 21.18605525173251891, 3.426801613781890854, -232.1183243183448894 ) ) ;
#5430 = ORIENTED_EDGE ( 'NONE', *, *, #17798, .T. ) ;
#5431 = CARTESIAN_POINT ( 'NONE',  ( 7.487558183825500535, -19.68056729374139380, -230.9679144533258466 ) ) ;
#5432 = ORIENTED_EDGE ( 'NONE', *, *, #4050, .T. ) ;
#5433 = CARTESIAN_POINT ( 'NONE',  ( 5.920964624126254350, -19.79845160325395526, -232.2234910544682123 ) ) ;
#5434 = CARTESIAN_POINT ( 'NONE',  ( -6.407569900110946293, 14.82357759665407215, -221.6203916094852957 ) ) ;
#5435 = ORIENTED_EDGE ( 'NONE', *, *, #18082, .F. ) ;
#5436 =( LENGTH_UNIT ( ) NAMED_UNIT ( * ) SI_UNIT ( .MILLI., .METRE. ) );
#5437 = VECTOR ( 'NONE', #10814, 1000.000000000000000 ) ;
#5438 = CARTESIAN_POINT ( 'NONE',  ( 17.68508104102419409, 23.41266195669770767, -227.5327139115408954 ) ) ;
#5439 = CARTESIAN_POINT ( 'NONE',  ( 28.36095019830170472, -8.296631283839911220, -225.2861439608085448 ) ) ;
#5440 = CARTESIAN_POINT ( 'NONE',  ( -9.606889355748592152, -11.26588727105406385, -229.9123324032181586 ) ) ;
#5441 = CARTESIAN_POINT ( 'NONE',  ( -0.6367083786117293531, -29.73461014436635708, -220.1383336929387724 ) ) ;
#5442 = CARTESIAN_POINT ( 'NONE',  ( -4.285397168228398890, 18.56782363833054106, -219.4990091916804715 ) ) ;
#5443 = CARTESIAN_POINT ( 'NONE',  ( 0.000000000000000000, 0.000000000000000000, 77.51594804401857175 ) ) ;
#5444 = CARTESIAN_POINT ( 'NONE',  ( 17.51175949430614409, 14.31829016556564937, -218.8195841045835550 ) ) ;
#5445 = CARTESIAN_POINT ( 'NONE',  ( -12.74846050492543625, 19.93509882904884734, -216.0172840992881049 ) ) ;
#5446 = CARTESIAN_POINT ( 'NONE',  ( -9.175187729848801155, 26.50888816229029743, -227.9285554593684253 ) ) ;
#5447 = ORIENTED_EDGE ( 'NONE', *, *, #198, .F. ) ;
#5448 = CIRCLE ( 'NONE', #4005, 17.50000000000000711 ) ;
#5449 = CARTESIAN_POINT ( 'NONE',  ( 9.880827190695510964, 24.82036951119805579, -218.1633337467656020 ) ) ;
#5450 = CARTESIAN_POINT ( 'NONE',  ( -20.92673740658815973, 5.672885432599523270, -219.1433548642331459 ) ) ;
#5451 = CARTESIAN_POINT ( 'NONE',  ( 25.30941179858102430, 8.661697827793627624, -216.7530520919057722 ) ) ;
#5452 = CARTESIAN_POINT ( 'NONE',  ( 13.60960062514055657, -26.18013421850907108, -225.9721930653775246 ) ) ;
#5453 = DIRECTION ( 'NONE',  ( 0.000000000000000000, 0.000000000000000000, -1.000000000000000000 ) ) ;
#5454 = ORIENTED_EDGE ( 'NONE', *, *, #6882, .T. ) ;
#5455 = CARTESIAN_POINT ( 'NONE',  ( -3.643097910890548796, 22.16888955197135047, -233.9701981029593298 ) ) ;
#5456 = CARTESIAN_POINT ( 'NONE',  ( 15.68576712525985251, -3.705577278900763716, -224.6781181500375908 ) ) ;
#5457 = CARTESIAN_POINT ( 'NONE',  ( 15.24934971233792957, -1.903332227395571508, -221.9416920766431076 ) ) ;
#5458 = CIRCLE ( 'NONE', #12440, 5.000000000000004441 ) ;
#5459 = CARTESIAN_POINT ( 'NONE',  ( 27.40550551777678123, 5.967061366481472895, -228.7463788799179554 ) ) ;
#5460 = CARTESIAN_POINT ( 'NONE',  ( -18.71530386740073126, -0.6857509888707814527, -217.6195632122020527 ) ) ;
#5461 = CARTESIAN_POINT ( 'NONE',  ( 5.982950994121768673, -14.58086824529316594, -231.1438280359330975 ) ) ;
#5462 = DIRECTION ( 'NONE',  ( 0.000000000000000000, 0.000000000000000000, 1.000000000000000000 ) ) ;
#5463 = CARTESIAN_POINT ( 'NONE',  ( -24.24202834850560606, 19.05981756344202438, -226.6980666352953335 ) ) ;
#5464 = CARTESIAN_POINT ( 'NONE',  ( -13.25293905438448405, 17.39325876214774524, -215.6628841494472510 ) ) ;
#5465 = VERTEX_POINT ( 'NONE', #15166 ) ;
#5466 = CARTESIAN_POINT ( 'NONE',  ( -14.68037037322036475, 3.441677802729143920, -220.1396515630443389 ) ) ;
#5467 = CARTESIAN_POINT ( 'NONE',  ( -12.60959727102843786, -12.64039607560028600, -218.2377899390859284 ) ) ;
#5468 = LINE ( 'NONE', #20882, #20953 ) ;
#5469 = CARTESIAN_POINT ( 'NONE',  ( 19.20300624114736721, 0.6066039755357417462, -231.5046416827383950 ) ) ;
#5470 = CARTESIAN_POINT ( 'NONE',  ( -12.44873260470819787, 7.411970124596155785, -229.4214091473984070 ) ) ;
#5471 = CARTESIAN_POINT ( 'NONE',  ( 1.780865994697476307, -30.77012162006053941, -222.8552464324424705 ) ) ;
#5472 = LINE ( 'NONE', #2207, #7054 ) ;
#5473 = AXIS2_PLACEMENT_3D ( 'NONE', #19796, #12846, #4379 ) ;
#5474 = CARTESIAN_POINT ( 'NONE',  ( -23.70658472240227255, 7.946283115275369013, 6.105263035233634561 ) ) ;
#5475 = CARTESIAN_POINT ( 'NONE',  ( 23.44063276014420794, 13.61134749381700182, -229.1061940987080732 ) ) ;
#5476 = CARTESIAN_POINT ( 'NONE',  ( -14.12265793148702464, 24.49085167151569919, -218.3312790639385241 ) ) ;
#5477 = CARTESIAN_POINT ( 'NONE',  ( -6.938893903907228378E-15, 0.000000000000000000, -224.9999999999999716 ) ) ;
#5478 = CARTESIAN_POINT ( 'NONE',  ( 15.70200226922815290, 22.14006925444000018, -227.8255507828836244 ) ) ;
#5479 = CARTESIAN_POINT ( 'NONE',  ( -3.968800477764047319, -14.91200208314756104, -226.8245746385127575 ) ) ;
#5480 = EDGE_LOOP ( 'NONE', ( #3232, #17739, #11618, #12233 ) ) ;
#5481 = CARTESIAN_POINT ( 'NONE',  ( -8.317278876689359279, 23.15034512777772235, -218.2935523245793092 ) ) ;
#5482 = CARTESIAN_POINT ( 'NONE',  ( -16.56270003954679382, 4.935922114544952777, -221.6503923146493378 ) ) ;
#5483 = CARTESIAN_POINT ( 'NONE',  ( -12.79639481117843935, 1.974037863663017589, -229.6094308443170746 ) ) ;
#5484 = ORIENTED_EDGE ( 'NONE', *, *, #8689, .F. ) ;
#5485 = CARTESIAN_POINT ( 'NONE',  ( -18.48279503042009964, -19.02624011246567548, -221.2510238762918107 ) ) ;
#5486 = CARTESIAN_POINT ( 'NONE',  ( 0.000000000000000000, 23.00000000000000000, -30.00000000000000000 ) ) ;
#5487 = ORIENTED_EDGE ( 'NONE', *, *, #17351, .F. ) ;
#5488 = CARTESIAN_POINT ( 'NONE',  ( 25.85597688020959239, 3.954559836939000039, -230.6766427064781624 ) ) ;
#5489 = CARTESIAN_POINT ( 'NONE',  ( 4.834917880317126659, -18.50358955815650219, -219.1181532354089256 ) ) ;
#5490 = CARTESIAN_POINT ( 'NONE',  ( 11.57669841200422134, 10.63052136557218574, -228.9489978335593889 ) ) ;
#5491 = CARTESIAN_POINT ( 'NONE',  ( -17.17400284685640344, 24.63223427531467280, -220.6313524368512162 ) ) ;
#5492 = AXIS2_PLACEMENT_3D ( 'NONE', #20986, #8964, #12337 ) ;
#5493 = AXIS2_PLACEMENT_3D ( 'NONE', #10834, #595, #12421 ) ;
#5494 = AXIS2_PLACEMENT_3D ( 'NONE', #5443, #5670, #19502 ) ;
#5495 = CARTESIAN_POINT ( 'NONE',  ( 13.40064012097826307, 2.532414129335418096, -221.5952957478750989 ) ) ;
#5496 = EDGE_CURVE ( 'NONE', #7331, #6505, #780, .T. ) ;
#5497 = CARTESIAN_POINT ( 'NONE',  ( 7.762960416026701616, 12.60702317161859121, -221.9096828323375235 ) ) ;
#5498 = DIRECTION ( 'NONE',  ( -0.000000000000000000, -0.000000000000000000, 1.000000000000000000 ) ) ;
#5499 = CARTESIAN_POINT ( 'NONE',  ( -5.420780812268581883, -12.08122409751860360, -226.5143039284326392 ) ) ;
#5500 = CARTESIAN_POINT ( 'NONE',  ( 10.99893791904045415, -12.61823049403341201, -218.3266956685045841 ) ) ;
#5501 = CARTESIAN_POINT ( 'NONE',  ( 2.100000000000000089, 0.000000000000000000, -105.0000000000000000 ) ) ;
#5502 = CARTESIAN_POINT ( 'NONE',  ( 0.000000000000000000, 0.000000000000000000, -77.51594804401857175 ) ) ;
#5503 = CARTESIAN_POINT ( 'NONE',  ( -13.55637112341987383, 4.614880311503475774, -231.8130385267184010 ) ) ;
#5504 = CARTESIAN_POINT ( 'NONE',  ( -17.58891219272264905, -6.833323493373833379, -229.9407564095759540 ) ) ;
#5505 = AXIS2_PLACEMENT_3D ( 'NONE', #1144, #20370, #15112 ) ;
#5506 = AXIS2_PLACEMENT_3D ( 'NONE', #13365, #9767, #16416 ) ;
#5507 = CARTESIAN_POINT ( 'NONE',  ( 24.52160379727246209, 5.049198597839295033, -215.7868787176665535 ) ) ;
#5508 = CARTESIAN_POINT ( 'NONE',  ( 2.535512286608554433, 13.86868953312499109, -224.9313928733152181 ) ) ;
#5509 = CARTESIAN_POINT ( 'NONE',  ( 2.601379523478754674, 17.36677895276155681, -230.4357129074444117 ) ) ;
#5510 = ORIENTED_EDGE ( 'NONE', *, *, #13136, .T. ) ;
#5511 = CARTESIAN_POINT ( 'NONE',  ( 20.22673842361927399, -24.21895433676095877, -222.6595898022596316 ) ) ;
#5512 = ORIENTED_EDGE ( 'NONE', *, *, #5705, .F. ) ;
#5513 = CARTESIAN_POINT ( 'NONE',  ( 12.85408565574548412, 7.821283853063205171, -223.1248833997948111 ) ) ;
#5514 = CARTESIAN_POINT ( 'NONE',  ( -17.15943377049709184, 17.77880916606822836, -233.2929083076029144 ) ) ;
#5515 = CARTESIAN_POINT ( 'NONE',  ( -21.01482965301294925, 6.368220028842532798, -231.7530032521518990 ) ) ;
#5516 = CARTESIAN_POINT ( 'NONE',  ( -14.76610802599379291, -3.249507257478274180, -230.1617063156812719 ) ) ;
#5517 = CARTESIAN_POINT ( 'NONE',  ( -23.49379658590067876, 11.46840048879614393, -217.2519070826072323 ) ) ;
#5518 = DIRECTION ( 'NONE',  ( -1.000000000000000000, 1.224646799147353454E-16, 0.000000000000000000 ) ) ;
#5519 = DIRECTION ( 'NONE',  ( 0.000000000000000000, 0.000000000000000000, 1.000000000000000000 ) ) ;
#5520 = FACE_OUTER_BOUND ( 'NONE', #22180, .T. ) ;
#5521 = AXIS2_PLACEMENT_3D ( 'NONE', #11789, #18655, #3216 ) ;
#5522 = CARTESIAN_POINT ( 'NONE',  ( -12.80756961294691010, 26.82110654133967387, -223.7464923486294026 ) ) ;
#5523 = CARTESIAN_POINT ( 'NONE',  ( 22.92330650806121639, 19.11387742755395180, -231.6463539987045976 ) ) ;
#5524 = CARTESIAN_POINT ( 'NONE',  ( 18.69835413980967687, -1.262199651413310031, -230.6153330080101966 ) ) ;
#5525 = CARTESIAN_POINT ( 'NONE',  ( -15.10499565381530118, -6.968761303117489980, -233.6783966751926869 ) ) ;
#5526 = CARTESIAN_POINT ( 'NONE',  ( -23.63383474287343589, -9.908731599815467916, -232.6396219513094081 ) ) ;
#5527 = CARTESIAN_POINT ( 'NONE',  ( -12.22073052649759184, 14.03927388329973525, -215.9097966823721606 ) ) ;
#5528 = CARTESIAN_POINT ( 'NONE',  ( -6.052919920376759855, -15.38051382379660836, -218.0337201863237624 ) ) ;
#5529 = CARTESIAN_POINT ( 'NONE',  ( 7.639528166734322667, 11.92751229241157596, -224.6077814063189635 ) ) ;
#5530 = CARTESIAN_POINT ( 'NONE',  ( 4.433847066018189231, -14.70588125837090487, -232.6468564462760469 ) ) ;
#5531 = DIRECTION ( 'NONE',  ( 0.000000000000000000, 0.000000000000000000, -1.000000000000000000 ) ) ;
#5532 = EDGE_CURVE ( 'NONE', #18185, #20995, #13591, .T. ) ;
#5533 = CARTESIAN_POINT ( 'NONE',  ( -15.36327147092456791, 5.453733681707060299, -220.0043800961136355 ) ) ;
#5534 = FILL_AREA_STYLE ('',( #14221 ) ) ;
#5535 = CARTESIAN_POINT ( 'NONE',  ( -8.752190949579933488, 24.25633523490762755, -230.6624101830059885 ) ) ;
#5536 = CARTESIAN_POINT ( 'NONE',  ( -27.92885697401080591, 6.962042978589167319, -220.9552227796709190 ) ) ;
#5537 = CARTESIAN_POINT ( 'NONE',  ( 18.04365516558436866, 6.721233635139160612, -218.4376093631473168 ) ) ;
#5538 = CARTESIAN_POINT ( 'NONE',  ( 24.49559427486850893, 14.86117239466233642, -230.3058416388274736 ) ) ;
#5539 = CARTESIAN_POINT ( 'NONE',  ( -7.879270980303660465, -15.58863178937888350, -218.8267223810934752 ) ) ;
#5540 = CARTESIAN_POINT ( 'NONE',  ( 18.99256614858759207, 26.22894869843687715, -224.5811130452664202 ) ) ;
#5541 = AXIS2_PLACEMENT_3D ( 'NONE', #22024, #6733, #4921 ) ;
#5542 = DIRECTION ( 'NONE',  ( 1.000000000000000000, 0.000000000000000000, 0.000000000000000000 ) ) ;
#5543 = CARTESIAN_POINT ( 'NONE',  ( -11.08668407991722304, -24.47826551258279082, -233.9784602105897875 ) ) ;
#5544 = CARTESIAN_POINT ( 'NONE',  ( -14.87932799058895128, 18.71706570923887369, -231.8731726670167745 ) ) ;
#5545 = ADVANCED_FACE ( 'NONE', ( #5018 ), #6604, .T. ) ;
#5546 = CARTESIAN_POINT ( 'NONE',  ( 11.98894270675143225, 20.38243841428667835, -233.2283128908360084 ) ) ;
#5547 = CARTESIAN_POINT ( 'NONE',  ( -18.67270963783218463, 15.11229250701181925, -218.9067109956068578 ) ) ;
#5548 = CARTESIAN_POINT ( 'NONE',  ( 2.660414182604129429, 28.99288898680367055, -232.5781547115647072 ) ) ;
#5549 = CARTESIAN_POINT ( 'NONE',  ( 25.40954707198727647, 2.077273811637330159, -219.3610170479527426 ) ) ;
#5550 = ORIENTED_EDGE ( 'NONE', *, *, #17171, .F. ) ;
#5551 = CARTESIAN_POINT ( 'NONE',  ( 12.31709745011784740, -23.08055702692190891, -220.7960250479738136 ) ) ;
#5552 = ORIENTED_EDGE ( 'NONE', *, *, #15025, .F. ) ;
#5553 = CARTESIAN_POINT ( 'NONE',  ( 7.739744183733028748, -12.54214339878522999, -227.5419174737939159 ) ) ;
#5554 = CARTESIAN_POINT ( 'NONE',  ( -1.796846813493219619, 26.08418332695505271, -220.7262848173578504 ) ) ;
#5555 = VERTEX_POINT ( 'NONE', #10208 ) ;
#5556 = DIRECTION ( 'NONE',  ( -0.000000000000000000, -0.000000000000000000, -1.000000000000000000 ) ) ;
#5557 = CIRCLE ( 'NONE', #13114, 5.000000000000004441 ) ;
#5558 = CARTESIAN_POINT ( 'NONE',  ( 18.76922974182421555, 13.12635134380198210, -217.8010375391909008 ) ) ;
#5559 = CARTESIAN_POINT ( 'NONE',  ( 17.00614511541963836, -1.958782916976874233, -219.4638360731791806 ) ) ;
#5560 = CARTESIAN_POINT ( 'NONE',  ( -16.05483997570105714, -7.226811045751038165, -218.5819178105544438 ) ) ;
#5561 = CARTESIAN_POINT ( 'NONE',  ( 2.967317674205219191, -16.40215926535219282, -217.6245344443522924 ) ) ;
#5562 = COLOUR_RGB ( '', 0.40784314, 0.44705882, 0.49803922) ;
#5563 = CARTESIAN_POINT ( 'NONE',  ( -8.467651734177735534, 23.23776955534497546, -231.2693664226804913 ) ) ;
#5564 = DIRECTION ( 'NONE',  ( 0.000000000000000000, 0.000000000000000000, -1.000000000000000000 ) ) ;
#5565 = CARTESIAN_POINT ( 'NONE',  ( 21.91535456744164279, 7.573568724377624406, -232.0371228855588868 ) ) ;
#5566 = CARTESIAN_POINT ( 'NONE',  ( -9.250876228778270871, 9.538614635316015722, -227.1332118982684563 ) ) ;
#5567 = CARTESIAN_POINT ( 'NONE',  ( -7.058999618647554541, 24.62458660126260312, -219.6630466582859356 ) ) ;
#5568 = ORIENTED_EDGE ( 'NONE', *, *, #3719, .T. ) ;
#5569 = CARTESIAN_POINT ( 'NONE',  ( 3.219568897812384645, 28.82511222849302257, -221.5626884747494216 ) ) ;
#5570 = CARTESIAN_POINT ( 'NONE',  ( -17.99155049254074612, 5.190958499132906745, -220.1449419322306937 ) ) ;
#5571 = CARTESIAN_POINT ( 'NONE',  ( 22.66015888791822519, 10.43487984001084534, -234.3950629709119937 ) ) ;
#5572 = CARTESIAN_POINT ( 'NONE',  ( 11.75796858304313375, -24.75965012883946414, -219.8219186532837455 ) ) ;
#5573 = DIRECTION ( 'NONE',  ( -1.000000000000000000, 0.000000000000000000, 0.000000000000000000 ) ) ;
#5574 = DIRECTION ( 'NONE',  ( -0.000000000000000000, -0.000000000000000000, 1.000000000000000000 ) ) ;
#5575 = CARTESIAN_POINT ( 'NONE',  ( 12.18657022793382794, 26.76558097653315471, -221.8882195427397335 ) ) ;
#5576 = CARTESIAN_POINT ( 'NONE',  ( 23.43833711860394686, -7.060024820847174531, -230.3984000052215606 ) ) ;
#5577 = FACE_OUTER_BOUND ( 'NONE', #5389, .T. ) ;
#5578 = CARTESIAN_POINT ( 'NONE',  ( 15.05360126642391450, 1.481754003466396963, -222.9454997252120734 ) ) ;
#5579 = AXIS2_PLACEMENT_3D ( 'NONE', #8457, #8669, #6525 ) ;
#5580 = CIRCLE ( 'NONE', #18165, 3.000000000000006217 ) ;
#5581 = CARTESIAN_POINT ( 'NONE',  ( 1.541778504653760429, -23.48174737203985529, -233.9922866444541967 ) ) ;
#5582 = PRESENTATION_STYLE_ASSIGNMENT (( #17412 ) ) ;
#5583 = CARTESIAN_POINT ( 'NONE',  ( -9.740348021262962064, 16.12529029871877384, -216.4361617420699702 ) ) ;
#5584 = CARTESIAN_POINT ( 'NONE',  ( -13.41298582792616934, 27.85383138489214616, -228.6457525465575884 ) ) ;
#5585 = ORIENTED_EDGE ( 'NONE', *, *, #13649, .F. ) ;
#5586 = CARTESIAN_POINT ( 'NONE',  ( -28.59157645096996347, 5.137867505054540374, -220.4667042235044505 ) ) ;
#5587 = CARTESIAN_POINT ( 'NONE',  ( -13.08346052978740914, -7.620079078745922274, -220.3923444982454498 ) ) ;
#5588 = CARTESIAN_POINT ( 'NONE',  ( -22.63401512838757057, 0.000000000000000000, -77.51594804401857175 ) ) ;
#5589 = DIRECTION ( 'NONE',  ( 0.000000000000000000, 0.000000000000000000, 1.000000000000000000 ) ) ;
#5590 = CARTESIAN_POINT ( 'NONE',  ( -26.74045434827795020, 12.41518252455047744, -220.4617428697642652 ) ) ;
#5591 = CARTESIAN_POINT ( 'NONE',  ( 7.717439423011566824, -15.08909893080012132, -230.2794769249191518 ) ) ;
#5592 = DIRECTION ( 'NONE',  ( 0.000000000000000000, -0.7999999999999999334, -0.5999999999999999778 ) ) ;
#5593 = CARTESIAN_POINT ( 'NONE',  ( 28.52435124311170966, 7.611291969169514005, -224.8315247833735384 ) ) ;
#5594 = CARTESIAN_POINT ( 'NONE',  ( -7.099035520468861549, 19.73710792467281649, -233.8745459908100770 ) ) ;
#5595 = FACE_OUTER_BOUND ( 'NONE', #4153, .T. ) ;
#5596 = CARTESIAN_POINT ( 'NONE',  ( 12.16813927252146144, 18.27141895336136912, -230.9123895730235745 ) ) ;
#5597 = CARTESIAN_POINT ( 'NONE',  ( 3.610394173775429039, -14.27701378914486874, -220.9234757326916281 ) ) ;
#5598 = EDGE_LOOP ( 'NONE', ( #9277, #10311 ) ) ;
#5599 = CARTESIAN_POINT ( 'NONE',  ( 2.464084843620814702, 29.35663482419208492, -227.0015060686748143 ) ) ;
#5600 = CARTESIAN_POINT ( 'NONE',  ( -9.222253059793434460, 13.27185325399938165, -229.0864811363590547 ) ) ;
#5601 = CARTESIAN_POINT ( 'NONE',  ( -18.16160515720599022, 12.42447964075808997, -216.1086293678848449 ) ) ;
#5602 = CARTESIAN_POINT ( 'NONE',  ( -18.79436262126649027, -19.56097393442729526, -222.1480387859219547 ) ) ;
#5603 = LINE ( 'NONE', #3577, #11109 ) ;
#5604 = VERTEX_POINT ( 'NONE', #16961 ) ;
#5605 = CARTESIAN_POINT ( 'NONE',  ( 22.05207439088920651, 1.190718621721708947, -218.4927357815377604 ) ) ;
#5606 = CARTESIAN_POINT ( 'NONE',  ( 8.467778565514151978, -25.57602835425881338, -228.7153423394380525 ) ) ;
#5607 = CARTESIAN_POINT ( 'NONE',  ( 15.89706143421296147, 10.57416387607782227, -218.3862415393350318 ) ) ;
#5608 = EDGE_CURVE ( 'NONE', #7196, #9986, #6530, .T. ) ;
#5609 = CARTESIAN_POINT ( 'NONE',  ( -21.02719846458807851, 18.12262440796364871, -218.0220709499931502 ) ) ;
#5610 = AXIS2_PLACEMENT_3D ( 'NONE', #16389, #6471, #11211 ) ;
#5611 = CARTESIAN_POINT ( 'NONE',  ( 29.21307215008108216, 4.139194015751272104, -229.9658791484231699 ) ) ;
#5612 = PRESENTATION_LAYER_ASSIGNMENT (  '', '', ( #21055 ) ) ;
#5613 = CARTESIAN_POINT ( 'NONE',  ( 0.9046320824004248085, 13.39785254849979701, -226.4815711199935890 ) ) ;
#5614 = CARTESIAN_POINT ( 'NONE',  ( 15.34286276367735979, 1.557318373440422565, -222.4358706187587416 ) ) ;
#5615 = CARTESIAN_POINT ( 'NONE',  ( -20.76924187596804217, -21.50248317380421170, -228.3679492147379335 ) ) ;
#5616 = CARTESIAN_POINT ( 'NONE',  ( 13.49882595795384255, -9.201056071450322449, -219.2439763087855908 ) ) ;
#5617 = CARTESIAN_POINT ( 'NONE',  ( -17.95451841861686049, 0.000000000000000000, -101.2940952255125922 ) ) ;
#5618 = CARTESIAN_POINT ( 'NONE',  ( 0.000000000000000000, 0.000000000000000000, 69.99999999999998579 ) ) ;
#5619 = CARTESIAN_POINT ( 'NONE',  ( -7.903959818038710061, 11.02445096303677552, -229.5951168968472871 ) ) ;
#5620 = CARTESIAN_POINT ( 'NONE',  ( -14.79915263310685347, -6.493660518011266092, -224.0818296219458716 ) ) ;
#5621 = CARTESIAN_POINT ( 'NONE',  ( -16.28025842329327944, 6.985656672962045732, -231.4191468057695715 ) ) ;
#5622 = CARTESIAN_POINT ( 'NONE',  ( 23.21336156720804667, 12.57464006230432574, -232.9346648124233070 ) ) ;
#5623 = CARTESIAN_POINT ( 'NONE',  ( 5.549682179574114471, 15.11687613544382280, -226.9959476502473308 ) ) ;
#5624 = ORIENTED_EDGE ( 'NONE', *, *, #15873, .T. ) ;
#5625 = CARTESIAN_POINT ( 'NONE',  ( 10.56552815906878529, -5.142824638143381755, -223.3550139360156663 ) ) ;
#5626 = ORIENTED_EDGE ( 'NONE', *, *, #11865, .F. ) ;
#5627 = CARTESIAN_POINT ( 'NONE',  ( 27.04607490430786854, 4.607450003618843049, -220.3758934308003461 ) ) ;
#5628 = CARTESIAN_POINT ( 'NONE',  ( -22.70558257617108922, 14.65737936663030538, -230.9775454010380997 ) ) ;
#5629 = EDGE_CURVE ( 'NONE', #15933, #6655, #6832, .T. ) ;
#5630 = CARTESIAN_POINT ( 'NONE',  ( -8.995433708001568718, 13.44373928221519243, -231.9251680978426577 ) ) ;
#5631 = CARTESIAN_POINT ( 'NONE',  ( -26.47652094774193188, -8.527600130219385122, -218.5932275281782324 ) ) ;
#5632 = CARTESIAN_POINT ( 'NONE',  ( -25.61997837663875188, 10.01664178086244483, -231.6711741719404074 ) ) ;
#5633 = CARTESIAN_POINT ( 'NONE',  ( 0.000000000000000000, 0.000000000000000000, -60.00000000000000000 ) ) ;
#5634 = CARTESIAN_POINT ( 'NONE',  ( 12.23284375931666013, 4.108221165122169616, -224.0993108960438462 ) ) ;
#5635 = CARTESIAN_POINT ( 'NONE',  ( -12.66290653391502907, 23.44312233264792411, -230.9359094203250606 ) ) ;
#5636 = CARTESIAN_POINT ( 'NONE',  ( 5.434119414999338815, 11.18343085245738777, -221.0450680983404936 ) ) ;
#5637 = CARTESIAN_POINT ( 'NONE',  ( 22.05207439088920651, 1.190718621721708947, -218.4927357815377604 ) ) ;
#5638 = CARTESIAN_POINT ( 'NONE',  ( -24.78729321827560739, -16.46449136890227294, -222.3867555963062443 ) ) ;
#5639 = CARTESIAN_POINT ( 'NONE',  ( 3.755480357635514022, 24.23367984900377436, -231.4105847235276201 ) ) ;
#5640 = CARTESIAN_POINT ( 'NONE',  ( 0.5120693878963755719, -30.63998626839889639, -227.9504769009175220 ) ) ;
#5641 = CARTESIAN_POINT ( 'NONE',  ( 17.60676319847677007, 21.31475060840986302, -219.8266339603936785 ) ) ;
#5642 = CARTESIAN_POINT ( 'NONE',  ( 21.11934605992122727, -20.14300392389669270, -232.3867613253685249 ) ) ;
#5643 = FACE_OUTER_BOUND ( 'NONE', #971, .T. ) ;
#5644 = CARTESIAN_POINT ( 'NONE',  ( -22.38347148959098121, 12.58966534755613687, -218.4978713241202399 ) ) ;
#5645 = DIRECTION ( 'NONE',  ( 0.000000000000000000, 0.000000000000000000, -1.000000000000000000 ) ) ;
#5646 = CARTESIAN_POINT ( 'NONE',  ( 27.54201077264015396, -3.286392687948289648, -218.1575117614944190 ) ) ;
#5647 = CARTESIAN_POINT ( 'NONE',  ( 11.39755372583812587, 20.40856199875060639, -231.2895618162029621 ) ) ;
#5648 = CARTESIAN_POINT ( 'NONE',  ( 22.16327814861754675, 7.634676377199016706, -234.0520676664821735 ) ) ;
#5649 = CARTESIAN_POINT ( 'NONE',  ( 16.07305932912010960, 0.9253679043337685872, -229.0409936706996064 ) ) ;
#5650 = CARTESIAN_POINT ( 'NONE',  ( -7.475691298859681311, -12.42146568352542779, -226.9176918848390017 ) ) ;
#5651 = EDGE_CURVE ( 'NONE', #15752, #12803, #19815, .T. ) ;
#5652 = CARTESIAN_POINT ( 'NONE',  ( 1.984991703947643904, 14.51738422979996912, -218.4500278854917781 ) ) ;
#5653 = CARTESIAN_POINT ( 'NONE',  ( 0.000000000000000000, 0.000000000000000000, -69.99999999999998579 ) ) ;
#5654 = CARTESIAN_POINT ( 'NONE',  ( -7.108809775916832940, -10.55228017211132929, -220.3225562754048212 ) ) ;
#5655 = CARTESIAN_POINT ( 'NONE',  ( -11.08731210905863840, 25.61052584666692766, -228.9953606804266997 ) ) ;
#5656 = CARTESIAN_POINT ( 'NONE',  ( 14.60728983664449387, 19.38727400458104455, -216.6381802409380555 ) ) ;
#5657 = ADVANCED_FACE ( 'NONE', ( #5577 ), #3552, .F. ) ;
#5658 = CARTESIAN_POINT ( 'NONE',  ( -15.82760502346409304, 5.624826830110399634, -227.5369622385896946 ) ) ;
#5659 = CARTESIAN_POINT ( 'NONE',  ( 4.065638640983322283, 32.08830473489500434, -226.0249194102539150 ) ) ;
#5660 = CARTESIAN_POINT ( 'NONE',  ( 22.37138132874926910, 6.723028048925958622, -217.7073806909121743 ) ) ;
#5661 = CARTESIAN_POINT ( 'NONE',  ( 10.17740660404977149, -19.92573511251913132, -219.0500883963018737 ) ) ;
#5662 = CARTESIAN_POINT ( 'NONE',  ( 13.38323588254664642, -24.59169381177348157, -229.6955247737395780 ) ) ;
#5663 = CARTESIAN_POINT ( 'NONE',  ( 0.1979841192334154676, 16.22068729745496540, -223.9539336445596973 ) ) ;
#5664 = DIRECTION ( 'NONE',  ( 0.000000000000000000, 0.000000000000000000, -1.000000000000000000 ) ) ;
#5665 = CARTESIAN_POINT ( 'NONE',  ( 15.01439307471096463, 1.118969480519667048, -226.7488225241675366 ) ) ;
#5666 = CARTESIAN_POINT ( 'NONE',  ( 20.89700225552940793, -4.547446057044195911, -232.3806459760843666 ) ) ;
#5667 = CARTESIAN_POINT ( 'NONE',  ( -18.44715843167851688, -19.86029123650958184, -231.9563062773970046 ) ) ;
#5668 = CARTESIAN_POINT ( 'NONE',  ( -8.257247207528708444, -26.39349301559143512, -217.9383130379005138 ) ) ;
#5669 = CARTESIAN_POINT ( 'NONE',  ( -2.806347010929339802, 19.90767250424812573, -230.9206976900916004 ) ) ;
#5670 = DIRECTION ( 'NONE',  ( -0.000000000000000000, -0.000000000000000000, 1.000000000000000000 ) ) ;
#5671 = CARTESIAN_POINT ( 'NONE',  ( 20.90058474538433231, 18.60939544422136294, -225.8027644507526475 ) ) ;
#5672 = CARTESIAN_POINT ( 'NONE',  ( -9.517741096562200909, 20.63709896626785678, -234.1036702156204967 ) ) ;
#5673 = CARTESIAN_POINT ( 'NONE',  ( -8.548213857283494477, 12.07277636836182211, -222.5354997492170241 ) ) ;
#5674 = ORIENTED_EDGE ( 'NONE', *, *, #2395, .F. ) ;
#5675 = CARTESIAN_POINT ( 'NONE',  ( 3.846342036506673612, 16.55327908958690131, -231.1358846258000597 ) ) ;
#5676 = CARTESIAN_POINT ( 'NONE',  ( 15.51129552754472307, 0.2180314803830030457, -231.3815478022924879 ) ) ;
#5677 = CARTESIAN_POINT ( 'NONE',  ( 18.59615491886314231, -0.2392802120807639710, -217.5848846836084078 ) ) ;
#5678 = CARTESIAN_POINT ( 'NONE',  ( 19.78534257568999166, -22.00365353819481840, -227.2618024355658974 ) ) ;
#5679 = DIRECTION ( 'NONE',  ( -0.000000000000000000, -0.000000000000000000, 1.000000000000000000 ) ) ;
#5680 = CYLINDRICAL_SURFACE ( 'NONE', #5492, 17.50000000000007816 ) ;
#5681 = CARTESIAN_POINT ( 'NONE',  ( 7.762960416026701616, 12.60702317161859121, -221.9096828323375235 ) ) ;
#5682 = CARTESIAN_POINT ( 'NONE',  ( 23.48259192634075632, -8.786327662478353062, -220.0176983167915807 ) ) ;
#5683 = CARTESIAN_POINT ( 'NONE',  ( 25.50000000000000000, -0.5000000000000000000, 0.000000000000000000 ) ) ;
#5684 = AXIS2_PLACEMENT_3D ( 'NONE', #2986, #3436, #20194 ) ;
#5685 = CARTESIAN_POINT ( 'NONE',  ( 7.088126259304779353, -19.25156530781288566, -233.7785425911077937 ) ) ;
#5686 = APPLICATION_CONTEXT ( 'automotive_design' ) ;
#5687 = CARTESIAN_POINT ( 'NONE',  ( -6.282398543089500187, 12.01615879894893801, -228.5121145169883903 ) ) ;
#5688 = CARTESIAN_POINT ( 'NONE',  ( -17.15943377049709184, 17.77880916606822836, -233.2929083076029144 ) ) ;
#5689 = CARTESIAN_POINT ( 'NONE',  ( -24.02434186778878455, 18.57431834865475651, -228.2662945587547370 ) ) ;
#5690 = CARTESIAN_POINT ( 'NONE',  ( -12.65123680455331190, -6.798726433138870817, -228.2089845657881710 ) ) ;
#5691 = DIRECTION ( 'NONE',  ( -1.083936797661035110E-15, -1.000000000000000000, 0.000000000000000000 ) ) ;
#5692 = CARTESIAN_POINT ( 'NONE',  ( -1.322875655532295136, 1.500000000000000000, -120.0000000000000142 ) ) ;
#5693 = CARTESIAN_POINT ( 'NONE',  ( -17.88126539071149779, 5.766250685202066961, -232.9050303536861293 ) ) ;
#5694 = CARTESIAN_POINT ( 'NONE',  ( 7.470327549107519616, -12.61959153319410909, -223.5186783388273568 ) ) ;
#5695 = CARTESIAN_POINT ( 'NONE',  ( 26.00000000000000000, 0.5000000000000000000, -6.000000000000000000 ) ) ;
#5696 = CARTESIAN_POINT ( 'NONE',  ( -10.51143808951550085, 11.41308718311005066, -231.3573069600382439 ) ) ;
#5697 = CARTESIAN_POINT ( 'NONE',  ( 27.94758519801750296, 7.894658480667867018, -227.3974864124137127 ) ) ;
#5698 = ADVANCED_FACE ( 'NONE', ( #21204 ), #5824, .F. ) ;
#5699 = CARTESIAN_POINT ( 'NONE',  ( -10.49339404011726984, 12.66576824096800991, -217.2681947942554643 ) ) ;
#5700 = CIRCLE ( 'NONE', #10037, 25.00000000000010303 ) ;
#5701 = DIRECTION ( 'NONE',  ( -1.000000000000000000, 0.000000000000000000, 0.000000000000000000 ) ) ;
#5702 = CARTESIAN_POINT ( 'NONE',  ( 16.49020573214642837, 22.44566021525517741, -224.7841662740084701 ) ) ;
#5703 = CARTESIAN_POINT ( 'NONE',  ( -2.820113134979321590, -27.38213018110698727, -220.3670599055385821 ) ) ;
#5704 = ORIENTED_EDGE ( 'NONE', *, *, #5532, .F. ) ;
#5705 = EDGE_CURVE ( 'NONE', #10234, #10093, #9075, .T. ) ;
#5706 = CARTESIAN_POINT ( 'NONE',  ( 3.192353461299334061, 22.13718518159985393, -217.1103300728619843 ) ) ;
#5707 = CARTESIAN_POINT ( 'NONE',  ( -11.79656379827575918, 10.43402410864828589, -226.0519616335988076 ) ) ;
#5708 = CARTESIAN_POINT ( 'NONE',  ( -20.80338291456855870, 18.97067006663518995, -230.9007617602332516 ) ) ;
#5709 = CARTESIAN_POINT ( 'NONE',  ( -13.11077419447928349, -11.05578789306379406, -228.2719546787038212 ) ) ;
#5710 = DIRECTION ( 'NONE',  ( 0.2588190451025213501, -3.169619151431772337E-17, 0.9659258262890680902 ) ) ;
#5711 = ORIENTED_EDGE ( 'NONE', *, *, #2519, .T. ) ;
#5712 = CARTESIAN_POINT ( 'NONE',  ( -14.68037037322036475, 3.441677802729143920, -220.1396515630443389 ) ) ;
#5713 = CARTESIAN_POINT ( 'NONE',  ( 0.3833872033527188639, -14.95856321834011915, -223.3240416624371107 ) ) ;
#5714 = CARTESIAN_POINT ( 'NONE',  ( 17.99029889091409018, 9.613712288440757092, -232.0298403238024036 ) ) ;
#5715 = CARTESIAN_POINT ( 'NONE',  ( 2.837900457371055563, 25.11342719071438978, -232.9871906064174709 ) ) ;
#5716 = CARTESIAN_POINT ( 'NONE',  ( -27.56397725925346975, 4.259055856374357241, -222.4951663284069241 ) ) ;
#5717 = CARTESIAN_POINT ( 'NONE',  ( 4.340445191644851874, 29.86837761166362881, -227.4879512554873315 ) ) ;
#5718 = CARTESIAN_POINT ( 'NONE',  ( 0.000000000000000000, 0.000000000000000000, -120.0000000000000142 ) ) ;
#5719 = CARTESIAN_POINT ( 'NONE',  ( -9.294226473174397540, -12.00440878504259601, -219.6990993854437875 ) ) ;
#5720 = CARTESIAN_POINT ( 'NONE',  ( 15.11994912051959972, -12.48385213956034079, -232.8079920308188377 ) ) ;
#5721 = FACE_OUTER_BOUND ( 'NONE', #1314, .T. ) ;
#5722 = CARTESIAN_POINT ( 'NONE',  ( 0.000000000000000000, 0.000000000000000000, 93.00000000000000000 ) ) ;
#5723 = CARTESIAN_POINT ( 'NONE',  ( -28.88770769694534479, 14.24820799418726480, -223.2044777450442155 ) ) ;
#5724 = CARTESIAN_POINT ( 'NONE',  ( -14.98971194994906853, -6.742389346827670771, -223.0360336987919823 ) ) ;
#5725 = CARTESIAN_POINT ( 'NONE',  ( -16.07193224038526580, 12.24477688577882439, -232.1409653212175499 ) ) ;
#5726 = CARTESIAN_POINT ( 'NONE',  ( 26.59731715018858011, 13.56210517473685329, -229.5787264587298466 ) ) ;
#5727 = CARTESIAN_POINT ( 'NONE',  ( -1.837924626891132229, 29.27703531260187475, -227.2344808100871774 ) ) ;
#5728 = ORIENTED_EDGE ( 'NONE', *, *, #2914, .F. ) ;
#5729 = CARTESIAN_POINT ( 'NONE',  ( 9.478576170506354259, -9.424747406754709900, -230.1309108789951949 ) ) ;
#5730 = CARTESIAN_POINT ( 'NONE',  ( 14.63113973005795643, 4.926264598692385199, -222.4866305912601945 ) ) ;
#5731 = CARTESIAN_POINT ( 'NONE',  ( -0.3984245442872364484, 11.77931270252508789, -223.1826369159892920 ) ) ;
#5732 = CIRCLE ( 'NONE', #21176, 1.000000000000000888 ) ;
#5733 = CARTESIAN_POINT ( 'NONE',  ( -5.191169535941942748, 31.49570301054888688, -227.4714364261087098 ) ) ;
#5734 = CARTESIAN_POINT ( 'NONE',  ( -25.32486352395475393, -3.505876693931964549, -233.0869506614649822 ) ) ;
#5735 = CARTESIAN_POINT ( 'NONE',  ( -17.88126539071149779, 5.766250685202066961, -232.9050303536861293 ) ) ;
#5736 = CARTESIAN_POINT ( 'NONE',  ( -3.344898002356346378, -14.20274344593240912, 93.00000000000001421 ) ) ;
#5737 = CARTESIAN_POINT ( 'NONE',  ( 23.36729170583618398, -5.500043712341283531, -232.1593072787115375 ) ) ;
#5738 = PRODUCT_RELATED_PRODUCT_CATEGORY ( 'part', '', ( #16780 ) ) ;
#5739 = CARTESIAN_POINT ( 'NONE',  ( -0.9851030586975465519, 19.34066537597387381, -233.8273485600932418 ) ) ;
#5740 = CARTESIAN_POINT ( 'NONE',  ( 29.08100487150598212, 12.14819438347179670, -226.9621620069135020 ) ) ;
#5741 = CARTESIAN_POINT ( 'NONE',  ( -25.29098058636142810, 5.014641116111857144, -217.4658967307323110 ) ) ;
#5742 = CARTESIAN_POINT ( 'NONE',  ( 15.85665641241444668, 18.24713744004561988, -217.7195292979064902 ) ) ;
#5743 = CARTESIAN_POINT ( 'NONE',  ( -28.57583275380518018, -9.842401781236429059, -222.4643230566485386 ) ) ;
#5744 = CARTESIAN_POINT ( 'NONE',  ( -2.665457046508036942, 16.94988614842223029, -218.7621057649994896 ) ) ;
#5745 = CARTESIAN_POINT ( 'NONE',  ( -5.420780812268581883, -12.08122409751860360, -226.5143039284326392 ) ) ;
#5746 = CARTESIAN_POINT ( 'NONE',  ( 9.586902571418640662, 24.43292817174309661, -231.9968623198229807 ) ) ;
#5747 = CARTESIAN_POINT ( 'NONE',  ( 3.784839621866231241, -12.46827349529254469, -229.8854786719440426 ) ) ;
#5748 = DIRECTION ( 'NONE',  ( -0.000000000000000000, 0.000000000000000000, -1.000000000000000000 ) ) ;
#5749 = CARTESIAN_POINT ( 'NONE',  ( -23.20103936322198024, 10.64725167743880085, -231.7714206262400864 ) ) ;
#5750 =( NAMED_UNIT ( * ) PLANE_ANGLE_UNIT ( ) SI_UNIT ( $, .RADIAN. ) );
#5751 = CARTESIAN_POINT ( 'NONE',  ( -27.94976817795961210, -4.610981384744690104, -229.1808304932418139 ) ) ;
#5752 = CARTESIAN_POINT ( 'NONE',  ( 3.433394806375676733, 19.92272173529517332, -219.3341428536850799 ) ) ;
#5753 = CARTESIAN_POINT ( 'NONE',  ( -16.74094048923576494, 16.03040267675914521, -217.9177456399057178 ) ) ;
#5754 = CARTESIAN_POINT ( 'NONE',  ( 28.51464931495100785, 5.422321182929326966, -223.8116416110474347 ) ) ;
#5755 = CARTESIAN_POINT ( 'NONE',  ( -12.44262610342426711, -20.67338498558408588, -232.3867413080560027 ) ) ;
#5756 = CARTESIAN_POINT ( 'NONE',  ( 24.19672885113291727, 10.99915907690374439, -233.6834417629405891 ) ) ;
#5757 = LINE ( 'NONE', #7576, #10191 ) ;
#5758 = CARTESIAN_POINT ( 'NONE',  ( -11.83854910565153062, -9.589341273415847411, -217.2594489226254098 ) ) ;
#5759 = CARTESIAN_POINT ( 'NONE',  ( 2.508382434586714282, 15.09451298870656011, -220.9010239894319625 ) ) ;
#5760 = CARTESIAN_POINT ( 'NONE',  ( 5.833753951408669813, 12.47745132051510453, -226.2508980627489450 ) ) ;
#5761 = EDGE_CURVE ( 'NONE', #17900, #8590, #14036, .T. ) ;
#5762 = CARTESIAN_POINT ( 'NONE',  ( -13.01542355754912172, 26.77630951171455820, -225.1545229496516356 ) ) ;
#5763 = CARTESIAN_POINT ( 'NONE',  ( -0.2269548806647709305, 12.31484924552052718, -228.6688778050056783 ) ) ;
#5764 = CARTESIAN_POINT ( 'NONE',  ( 23.64727379217503866, 9.907944788639682088, -232.0643337313508709 ) ) ;
#5765 = CARTESIAN_POINT ( 'NONE',  ( 7.956221944547102964, -16.14435353399512252, -220.6073666753051441 ) ) ;
#5766 = CARTESIAN_POINT ( 'NONE',  ( 6.260833139380572732, -16.02228513277848876, -219.5457089733663736 ) ) ;
#5767 = CARTESIAN_POINT ( 'NONE',  ( -6.564517230509238743, 23.65597541655194647, -219.1225629381441991 ) ) ;
#5768 = EDGE_LOOP ( 'NONE', ( #8989, #3794, #2006, #11869 ) ) ;
#5769 = CARTESIAN_POINT ( 'NONE',  ( 0.000000000000000000, 0.000000000000000000, -78.50000000000000000 ) ) ;
#5770 = CARTESIAN_POINT ( 'NONE',  ( 14.22574309452842733, 4.476723532073429546, -225.5862451792618231 ) ) ;
#5771 = CARTESIAN_POINT ( 'NONE',  ( 14.90979066288448429, -1.927202206923867234, -222.7790985701595616 ) ) ;
#5772 = CARTESIAN_POINT ( 'NONE',  ( -14.78079095050690661, -5.416970230978240153, -229.7193632018645246 ) ) ;
#5773 = CARTESIAN_POINT ( 'NONE',  ( 1.780803752597676537, -13.83832444325970101, -229.2250779460899537 ) ) ;
#5774 = CARTESIAN_POINT ( 'NONE',  ( 6.608541902967795423, 16.43938546752961116, -220.2982508316308952 ) ) ;
#5775 = DIRECTION ( 'NONE',  ( -0.000000000000000000, -0.000000000000000000, -1.000000000000000000 ) ) ;
#5776 = CARTESIAN_POINT ( 'NONE',  ( -11.78887577478644566, 1.715692547334320084, -224.3106172711415525 ) ) ;
#5777 = CARTESIAN_POINT ( 'NONE',  ( -14.73016414256368911, 22.23431809695627237, -217.1425123644553707 ) ) ;
#5778 = CARTESIAN_POINT ( 'NONE',  ( 3.281983756374524663, 15.83593597903271721, -223.8697822987047346 ) ) ;
#5779 = CARTESIAN_POINT ( 'NONE',  ( 29.76850351104168979, -8.061840962539296385, -221.9850081079297581 ) ) ;
#5780 = ORIENTED_EDGE ( 'NONE', *, *, #6636, .T. ) ;
#5782 = EDGE_CURVE ( 'NONE', #6063, #18247, #19467, .T. ) ;
#5781 = EDGE_LOOP ( 'NONE', ( #20629, #3437, #20188, #5552 ) ) ;
#5783 = CARTESIAN_POINT ( 'NONE',  ( 13.20340559785743828, 9.575208899273587093, -218.1210831379648312 ) ) ;
#5784 = CARTESIAN_POINT ( 'NONE',  ( -14.47418542577149836, 8.806675964858893479, -228.0010566307936699 ) ) ;
#5785 = CARTESIAN_POINT ( 'NONE',  ( 13.70635042947887428, -1.390919209824193592, -225.3477037409554953 ) ) ;
#5786 = CARTESIAN_POINT ( 'NONE',  ( -1.432270239486107766, -17.91381153981195951, -219.1344183636291802 ) ) ;
#5787 = CARTESIAN_POINT ( 'NONE',  ( 0.000000000000000000, 0.000000000000000000, -77.51594804401857175 ) ) ;
#5788 = VERTEX_POINT ( 'NONE', #10867 ) ;
#5789 = CARTESIAN_POINT ( 'NONE',  ( 4.389496648589924277, 14.47660514356954131, -220.6151178996808540 ) ) ;
#5790 = CARTESIAN_POINT ( 'NONE',  ( 25.46431111394153390, -2.048831322092446783, -230.3135391428295975 ) ) ;
#5791 = DIRECTION ( 'NONE',  ( 0.000000000000000000, 1.000000000000000000, 0.000000000000000000 ) ) ;
#5792 = CARTESIAN_POINT ( 'NONE',  ( -0.8413160509385254615, -28.71376977722865931, -218.8117683208458288 ) ) ;
#5793 = APPLICATION_PROTOCOL_DEFINITION ( 'draft international standard', 'automotive_design', 1998, #4828 ) ;
#5794 = CARTESIAN_POINT ( 'NONE',  ( -13.83274569775339202, 16.20364235096346661, -234.0851861771356539 ) ) ;
#5795 = CARTESIAN_POINT ( 'NONE',  ( -5.543543819386913540, 14.51457927969963713, -217.3847528063896846 ) ) ;
#5796 = CARTESIAN_POINT ( 'NONE',  ( -13.55591840520136770, 8.363404288414606924, -231.2690188357804857 ) ) ;
#5797 = CARTESIAN_POINT ( 'NONE',  ( -19.65071121466273496, -22.30814805266854606, -225.1308016072272267 ) ) ;
#5798 = CARTESIAN_POINT ( 'NONE',  ( -21.63401512838747820, 0.000000000000000000, 77.51594804401857175 ) ) ;
#5799 = CARTESIAN_POINT ( 'NONE',  ( -23.00000000000006750, -1.237926774615798086E-16, -10.00000000000000000 ) ) ;
#5800 = CARTESIAN_POINT ( 'NONE',  ( -5.807479211365208727, 19.77444019604324410, -216.0778658752277863 ) ) ;
#5801 = CARTESIAN_POINT ( 'NONE',  ( 3.085658278449291192, -27.83354332032029888, -231.5475985764057043 ) ) ;
#5802 = DIRECTION ( 'NONE',  ( 1.000000000000000000, 0.000000000000000000, 0.000000000000000000 ) ) ;
#5803 = CARTESIAN_POINT ( 'NONE',  ( -15.82069055112642353, 8.315535108674763976, -217.2800172218543935 ) ) ;
#5804 = AXIS2_PLACEMENT_3D ( 'NONE', #11415, #2303, #9187 ) ;
#5805 = CARTESIAN_POINT ( 'NONE',  ( -18.09994298044773942, 1.383435435878707320, -215.7801353739235708 ) ) ;
#5806 = CARTESIAN_POINT ( 'NONE',  ( -1.707778556226592581, 19.51307486516442680, -232.5708079709245055 ) ) ;
#5807 = CARTESIAN_POINT ( 'NONE',  ( 13.55929460187270053, 0.3562519042583365270, -227.9787723277739246 ) ) ;
#5808 = CARTESIAN_POINT ( 'NONE',  ( 20.59763700141659015, 7.383112456150029423, -232.0722244125682039 ) ) ;
#5809 = CARTESIAN_POINT ( 'NONE',  ( -11.76273268715550913, -21.77324546118368787, -230.3967548854103313 ) ) ;
#5810 = EDGE_CURVE ( 'NONE', #7856, #13407, #365, .T. ) ;
#5811 = ORIENTED_EDGE ( 'NONE', *, *, #6066, .T. ) ;
#5812 = CARTESIAN_POINT ( 'NONE',  ( -4.855966894080006035, 26.75753167227873064, -230.1547293463117114 ) ) ;
#5813 = CARTESIAN_POINT ( 'NONE',  ( -9.007976471255481954, 12.60968992764439633, -227.9367755778692981 ) ) ;
#5814 = CARTESIAN_POINT ( 'NONE',  ( -20.04070223234628756, 18.12164545743767263, -231.9292141396248610 ) ) ;
#5815 = CIRCLE ( 'NONE', #15527, 3.000000000000002665 ) ;
#5816 = ORIENTED_EDGE ( 'NONE', *, *, #17196, .T. ) ;
#5817 = CARTESIAN_POINT ( 'NONE',  ( -12.84507615163359873, -10.94093879717347129, -227.8208865714805142 ) ) ;
#5818 = CARTESIAN_POINT ( 'NONE',  ( -6.938893903907228378E-15, 0.000000000000000000, -224.9999999999999716 ) ) ;
#5819 = EDGE_LOOP ( 'NONE', ( #17403, #18927 ) ) ;
#5820 = CARTESIAN_POINT ( 'NONE',  ( -26.02440924314744919, 2.824604386891162111, -232.0644005296583430 ) ) ;
#5821 = CARTESIAN_POINT ( 'NONE',  ( 2.864019721262919926, -25.46936398327173379, -230.7696170053991978 ) ) ;
#5822 = CARTESIAN_POINT ( 'NONE',  ( 15.33737796850231305, 13.57479350230705428, -232.3313557812109025 ) ) ;
#5823 = CARTESIAN_POINT ( 'NONE',  ( 0.9046320824004248085, 13.39785254849979701, -226.4815711199935890 ) ) ;
#5824 = TOROIDAL_SURFACE ( 'NONE', #7991, 22.56777165119825668, 3.000000000000000000 ) ;
#5825 = EDGE_CURVE ( 'NONE', #20879, #12254, #6862, .T. ) ;
#5826 = CARTESIAN_POINT ( 'NONE',  ( -25.19195624009214640, 10.50676406307063182, -220.0954552869889937 ) ) ;
#5827 = CARTESIAN_POINT ( 'NONE',  ( 15.88965480228581839, 12.37830464553330678, -233.8570207506254235 ) ) ;
#5828 = VECTOR ( 'NONE', #231, 1000.000000000000000 ) ;
#5829 = CARTESIAN_POINT ( 'NONE',  ( 14.54149994592679107, 8.070685273005897997, -229.7292930672863349 ) ) ;
#5830 = CARTESIAN_POINT ( 'NONE',  ( 0.000000000000000000, 0.000000000000000000, 75.01817430661621700 ) ) ;
#5831 = CARTESIAN_POINT ( 'NONE',  ( -12.14186164972853810, -9.217338937739926408, -220.4665480714278374 ) ) ;
#5832 = CARTESIAN_POINT ( 'NONE',  ( 1.836136847161299990, -12.84546502099244591, -226.1727064218434293 ) ) ;
#5833 = DIRECTION ( 'NONE',  ( 1.000000000000000000, 0.000000000000000000, 0.000000000000000000 ) ) ;
#5834 = CARTESIAN_POINT ( 'NONE',  ( -23.00000000000008882, 0.000000000000000000, 75.00000000000000000 ) ) ;
#5835 = CARTESIAN_POINT ( 'NONE',  ( -4.450022810944913587, 12.45400981846350597, -225.2098051417536340 ) ) ;
#5836 = CARTESIAN_POINT ( 'NONE',  ( 22.41656803062015157, -8.700679067278056067, -214.8043567724421337 ) ) ;
#5837 = CARTESIAN_POINT ( 'NONE',  ( 10.12956299421491302, 11.38773431477224385, -230.3175791991728829 ) ) ;
#5838 = CARTESIAN_POINT ( 'NONE',  ( 8.856360819293511710, 14.24139612884802553, -227.7731680686805475 ) ) ;
#5839 = EDGE_LOOP ( 'NONE', ( #2522, #2219, #4233, #22152 ) ) ;
#5840 = CARTESIAN_POINT ( 'NONE',  ( 10.41909793732091494, -5.130961835214151279, -225.2553394319931783 ) ) ;
#5841 = CARTESIAN_POINT ( 'NONE',  ( 20.23125423326388628, 7.836699765464857137, -217.8891354894872450 ) ) ;
#5842 = AXIS2_PLACEMENT_3D ( 'NONE', #11755, #17155, #1731 ) ;
#5843 = CARTESIAN_POINT ( 'NONE',  ( -5.568057711815838751, 28.69723585065299076, -232.1518503103610271 ) ) ;
#5844 = CARTESIAN_POINT ( 'NONE',  ( -7.812160407601123069, 10.19183344000749081, -223.8148904943605828 ) ) ;
#5845 = CARTESIAN_POINT ( 'NONE',  ( -16.30907414568449454, -3.310091733494833655, -231.8954501777161283 ) ) ;
#5846 = CARTESIAN_POINT ( 'NONE',  ( -18.09776816382430908, 23.50806826204562583, -229.9568677523880638 ) ) ;
#5847 = CARTESIAN_POINT ( 'NONE',  ( -0.2467007162552578292, -14.49943138577569357, 93.00000000000002842 ) ) ;
#5848 = CARTESIAN_POINT ( 'NONE',  ( 27.36047156164216787, -8.591464759722228450, -221.3690063136810977 ) ) ;
#5849 = CARTESIAN_POINT ( 'NONE',  ( -6.496078068315311427, 23.46891392553531119, -233.1042179568201220 ) ) ;
#5850 = CARTESIAN_POINT ( 'NONE',  ( 29.33969601628096768, 11.98971187598327504, -225.2039690377576733 ) ) ;
#5851 = CARTESIAN_POINT ( 'NONE',  ( -12.44873260470819787, 7.411970124596155785, -229.4214091473984070 ) ) ;
#5852 = CARTESIAN_POINT ( 'NONE',  ( 11.82943521288609823, 27.58963564415041247, -226.1180395413371400 ) ) ;
#5853 = AXIS2_PLACEMENT_3D ( 'NONE', #13532, #22072, #17021 ) ;
#5854 = AXIS2_PLACEMENT_3D ( 'NONE', #20104, #4808, #20213 ) ;
#5855 = PLANE ( 'NONE',  #4043 ) ;
#5856 = CARTESIAN_POINT ( 'NONE',  ( -1.316322971969275502, 14.13179993441458215, -224.9782367179667233 ) ) ;
#5857 = CARTESIAN_POINT ( 'NONE',  ( -13.67406442719345883, -9.319000780081536206, -231.1492214949047934 ) ) ;
#5858 = CARTESIAN_POINT ( 'NONE',  ( 8.689059922489732912, 15.18271246186214363, -218.7354841152034908 ) ) ;
#5859 = CARTESIAN_POINT ( 'NONE',  ( 6.910796951316678260, -9.495606915386650471, -226.6778026831113380 ) ) ;
#5860 = CARTESIAN_POINT ( 'NONE',  ( -6.938893903907228378E-15, 0.000000000000000000, -224.9999999999999716 ) ) ;
#5861 = CARTESIAN_POINT ( 'NONE',  ( -18.94992041651601156, 14.87246523864368974, -232.0280096192260828 ) ) ;
#5862 = CARTESIAN_POINT ( 'NONE',  ( 24.57161139520042781, -7.530326316930160857, -232.9949629211864419 ) ) ;
#5863 = CARTESIAN_POINT ( 'NONE',  ( 7.508136856874425114, 24.19512352541684663, -230.0608033085341617 ) ) ;
#5864 = CARTESIAN_POINT ( 'NONE',  ( -15.11329978779464689, 11.41628732213579411, -231.7124318929555500 ) ) ;
#5865 = CARTESIAN_POINT ( 'NONE',  ( -15.57331739480619248, 4.297375044201914740, -216.4079605712025511 ) ) ;
#5866 = CARTESIAN_POINT ( 'NONE',  ( -20.91998163778511355, -19.58520498255836628, -224.2692832511962990 ) ) ;
#5867 = CARTESIAN_POINT ( 'NONE',  ( 17.65694480011521250, 15.62497337860048674, -235.2008064134603273 ) ) ;
#5868 = CIRCLE ( 'NONE', #131, 3.000000000000002665 ) ;
#5869 = AXIS2_PLACEMENT_3D ( 'NONE', #12923, #992, #7866 ) ;
#5870 = DIRECTION ( 'NONE',  ( 0.000000000000000000, -0.7999999999999997113, 0.6000000000000004219 ) ) ;
#5871 = CARTESIAN_POINT ( 'NONE',  ( -15.80613518906033121, -10.93105391054944597, -234.9065563738643903 ) ) ;
#5872 = CARTESIAN_POINT ( 'NONE',  ( -4.224287562409271501, 29.03635716824519264, -224.1823526280761882 ) ) ;
#5873 = EDGE_CURVE ( 'NONE', #19507, #13805, #10857, .T. ) ;
#5874 = CARTESIAN_POINT ( 'NONE',  ( 13.30790133003807441, 0.6370684082013071681, -222.3495379725305270 ) ) ;
#5875 = CARTESIAN_POINT ( 'NONE',  ( -8.985448925281199095, 11.82743561134668475, -224.1067108988273162 ) ) ;
#5876 = ADVANCED_BREP_SHAPE_REPRESENTATION ( '', ( #6798, #6677 ), #16347 ) ;
#5877 = CARTESIAN_POINT ( 'NONE',  ( -4.619644865335168049, 14.75104250038670450, -232.3086264397671812 ) ) ;
#5878 = CARTESIAN_POINT ( 'NONE',  ( -15.23434562258889891, -0.4010941804143903222, -220.4743703065900036 ) ) ;
#5879 = VERTEX_POINT ( 'NONE', #14152 ) ;
#5880 = CARTESIAN_POINT ( 'NONE',  ( -4.241635020808209866, -19.61639137582426429, -216.9458228475819226 ) ) ;
#5881 = ORIENTED_EDGE ( 'NONE', *, *, #3565, .F. ) ;
#5882 = CARTESIAN_POINT ( 'NONE',  ( 11.12240951639491549, -23.90857633046665853, -218.9373339142375130 ) ) ;
#5883 = DIRECTION ( 'NONE',  ( -1.224646799147353207E-16, 1.000000000000000000, 0.000000000000000000 ) ) ;
#5884 = CARTESIAN_POINT ( 'NONE',  ( 22.66390650824515873, 11.48342577402021725, -231.3155567808436217 ) ) ;
#5885 = CARTESIAN_POINT ( 'NONE',  ( 29.12543877365354916, -1.475122899492763873, -224.0746120762670444 ) ) ;
#5886 = CARTESIAN_POINT ( 'NONE',  ( -8.491902988188710921, -10.37035003683405066, -223.9502466269643435 ) ) ;
#5887 = CARTESIAN_POINT ( 'NONE',  ( -18.64257584594551531, -16.66392856591270899, -217.1407738418131999 ) ) ;
#5888 = CARTESIAN_POINT ( 'NONE',  ( 4.152856881432678726, 16.71326706899027670, -228.3712188091315909 ) ) ;
#5889 = CARTESIAN_POINT ( 'NONE',  ( 0.000000000000000000, -23.00000000000000000, -75.00000000000000000 ) ) ;
#5890 = CARTESIAN_POINT ( 'NONE',  ( -15.00242079508237936, 7.335218745534954898, -232.9526071471669013 ) ) ;
#5891 = VECTOR ( 'NONE', #13827, 1000.000000000000000 ) ;
#5892 = CARTESIAN_POINT ( 'NONE',  ( -11.33137429837660193, 27.25022425932026238, -230.1650924901870212 ) ) ;
#5893 = CARTESIAN_POINT ( 'NONE',  ( -2.993956627714193353, 22.04778837082692178, -231.1741803919495339 ) ) ;
#5894 = CARTESIAN_POINT ( 'NONE',  ( 27.04962740251871978, -7.854494666110665158, -217.8595067830158882 ) ) ;
#5895 = ORIENTED_EDGE ( 'NONE', *, *, #18322, .T. ) ;
#5896 = CARTESIAN_POINT ( 'NONE',  ( 10.88376588832297287, 7.577514201227793400, -222.7215714477710833 ) ) ;
#5897 = EDGE_CURVE ( 'NONE', #15809, #68, #82, .T. ) ;
#5898 = CARTESIAN_POINT ( 'NONE',  ( -15.77374768176864173, 20.07639682234129097, -218.6858893794192795 ) ) ;
#5899 = CARTESIAN_POINT ( 'NONE',  ( 11.17228388010293649, 5.622653638471959425, -222.3672781564363845 ) ) ;
#5900 = CARTESIAN_POINT ( 'NONE',  ( 0.2799207934783670693, -28.72270877262613453, -227.3216717588132667 ) ) ;
#5901 = DIRECTION ( 'NONE',  ( -0.000000000000000000, -0.000000000000000000, 1.000000000000000000 ) ) ;
#5902 = DIRECTION ( 'NONE',  ( 0.000000000000000000, 0.000000000000000000, 1.000000000000000000 ) ) ;
#5903 = CARTESIAN_POINT ( 'NONE',  ( 7.639528166734322667, 11.92751229241157596, -224.6077814063189635 ) ) ;
#5904 = CARTESIAN_POINT ( 'NONE',  ( 17.50516624540364319, -11.67908417450482794, -218.9956384138364740 ) ) ;
#5905 = CARTESIAN_POINT ( 'NONE',  ( 0.000000000000000000, 0.000000000000000000, -105.0000000000000000 ) ) ;
#5906 = CARTESIAN_POINT ( 'NONE',  ( -15.46269062504165781, -26.67469327287815517, -225.2085449711190677 ) ) ;
#5907 = APPLICATION_PROTOCOL_DEFINITION ( 'draft international standard', 'automotive_design', 1998, #19060 ) ;
#5908 = CARTESIAN_POINT ( 'NONE',  ( 5.248230734842167955, 23.54336384919183445, -216.8914391693808739 ) ) ;
#5909 = CIRCLE ( 'NONE', #4830, 4.100000000000000533 ) ;
#5910 = CARTESIAN_POINT ( 'NONE',  ( 4.213939275857851108, 16.79797086795582928, -215.8378124706958943 ) ) ;
#5911 = ORIENTED_EDGE ( 'NONE', *, *, #9624, .F. ) ;
#5912 = CARTESIAN_POINT ( 'NONE',  ( -12.74846050492543625, 19.93509882904884734, -216.0172840992881049 ) ) ;
#5913 = CARTESIAN_POINT ( 'NONE',  ( -14.01584329375060456, -3.774282517739922405, -220.6818330080343173 ) ) ;
#5914 = CARTESIAN_POINT ( 'NONE',  ( 13.12488928717151637, 1.784773061176598909E-15, -103.0000000000000000 ) ) ;
#5915 = CARTESIAN_POINT ( 'NONE',  ( 0.000000000000000000, 0.000000000000000000, -75.00000000000000000 ) ) ;
#5916 = CARTESIAN_POINT ( 'NONE',  ( -15.66530208164916260, 23.23467148471576849, -218.1250122661128046 ) ) ;
#5917 = CARTESIAN_POINT ( 'NONE',  ( 3.671249956548685578, -18.86103685443826805, -233.0640024924723548 ) ) ;
#5918 = DIRECTION ( 'NONE',  ( 0.000000000000000000, 0.000000000000000000, -1.000000000000000000 ) ) ;
#5919 = CARTESIAN_POINT ( 'NONE',  ( -22.04257564474043818, 18.72061943465525857, -219.1781831295219263 ) ) ;
#5920 = CARTESIAN_POINT ( 'NONE',  ( 22.24262848503957812, 2.205713500382371794, -232.7243927205662430 ) ) ;
#5921 = CARTESIAN_POINT ( 'NONE',  ( 5.720314275582434327, 25.17872937134267630, -219.7530083620574430 ) ) ;
#5922 = CARTESIAN_POINT ( 'NONE',  ( 0.000000000000000000, 0.000000000000000000, -74.48236190979496030 ) ) ;
#5923 = CARTESIAN_POINT ( 'NONE',  ( 14.04819512851487673, 6.831178966487911453, -222.6676118107292552 ) ) ;
#5924 = CARTESIAN_POINT ( 'NONE',  ( -9.501265986711061373, -18.16888683615402300, -230.9326763462221948 ) ) ;
#5925 = ORIENTED_EDGE ( 'NONE', *, *, #8488, .T. ) ;
#5926 = CARTESIAN_POINT ( 'NONE',  ( 17.31940731551425827, 24.90170669671083914, -222.9868986272316533 ) ) ;
#5927 = CARTESIAN_POINT ( 'NONE',  ( -6.255852670334142829, 13.96671599789818252, -220.4426911866496823 ) ) ;
#5928 = CARTESIAN_POINT ( 'NONE',  ( -11.05707385098054729, 9.265475627845670914, -220.9763772784480693 ) ) ;
#5929 = CARTESIAN_POINT ( 'NONE',  ( 29.82766783012230505, -1.714217446056379934, -229.3564438616236316 ) ) ;
#5930 = CARTESIAN_POINT ( 'NONE',  ( 0.000000000000000000, 23.00000000000006040, -69.99999999999998579 ) ) ;
#5931 = CIRCLE ( 'NONE', #3415, 21.80000000000008598 ) ;
#5932 = ORIENTED_EDGE ( 'NONE', *, *, #5810, .T. ) ;
#5933 = CARTESIAN_POINT ( 'NONE',  ( 15.57986488780344736, -0.6155558446892130942, -225.2777919203616932 ) ) ;
#5934 = CARTESIAN_POINT ( 'NONE',  ( -7.509561119170069077, -14.53281319394193538, -217.7574163112487042 ) ) ;
#5935 = CARTESIAN_POINT ( 'NONE',  ( 14.38487221378403014, 1.734196266254829588, -227.4481254949095330 ) ) ;
#5936 = CARTESIAN_POINT ( 'NONE',  ( 2.008896548638861024, 20.64812324442097591, -233.5818019448501843 ) ) ;
#5937 = DIRECTION ( 'NONE',  ( -1.000000000000000000, 0.000000000000000000, 0.000000000000000000 ) ) ;
#5938 = CARTESIAN_POINT ( 'NONE',  ( -24.05551141223569545, 2.266836731622281498, -230.7594878221277384 ) ) ;
#5939 = ADVANCED_FACE ( 'NONE', ( #19305 ), #14769, .F. ) ;
#5940 = CARTESIAN_POINT ( 'NONE',  ( 7.739849882373770917, 11.59357455229016409, -219.5521933286238720 ) ) ;
#5941 = CARTESIAN_POINT ( 'NONE',  ( 26.29894631880581812, 12.29609390142961090, -226.3100047295820332 ) ) ;
#5942 = LINE ( 'NONE', #13149, #19177 ) ;
#5943 = CARTESIAN_POINT ( 'NONE',  ( -24.53655852862112496, -9.573911656693818273, -234.4221496410225143 ) ) ;
#5944 = VECTOR ( 'NONE', #311, 1000.000000000000000 ) ;
#5945 = CARTESIAN_POINT ( 'NONE',  ( -12.04756914620937636, -13.80987496524771885, -232.8991007102355582 ) ) ;
#5946 = CARTESIAN_POINT ( 'NONE',  ( 1.127544764349826867, -27.89617517048659323, -231.9509945439240823 ) ) ;
#5947 = DIRECTION ( 'NONE',  ( -1.000000000000000000, 0.000000000000000000, 0.000000000000000000 ) ) ;
#5948 = DIRECTION ( 'NONE',  ( 0.000000000000000000, 0.000000000000000000, 1.000000000000000000 ) ) ;
#5949 = CARTESIAN_POINT ( 'NONE',  ( -1.336753021691559962, 16.04398320409420720, -230.2310715620304507 ) ) ;
#5950 = CARTESIAN_POINT ( 'NONE',  ( 11.84677440217253341, -6.023754617643652054, -230.4469913264703962 ) ) ;
#5951 = CARTESIAN_POINT ( 'NONE',  ( 14.31589812732703670, -5.349901619299376243, -221.2752230612865105 ) ) ;
#5952 = CARTESIAN_POINT ( 'NONE',  ( -18.04772061096520375, 5.916925414182395038, -217.8829197293425750 ) ) ;
#5953 = CARTESIAN_POINT ( 'NONE',  ( 11.64932556965463561, 7.668732705389711413, -229.0406978839571366 ) ) ;
#5954 = CARTESIAN_POINT ( 'NONE',  ( 10.48640380280471618, 25.27581435651469022, -227.8976696013017715 ) ) ;
#5955 = ORIENTED_EDGE ( 'NONE', *, *, #3361, .F. ) ;
#5956 = CARTESIAN_POINT ( 'NONE',  ( 4.565444334214069144, -15.90021673156186388, -218.4840512714275462 ) ) ;
#5957 = CARTESIAN_POINT ( 'NONE',  ( -7.677656142228050484, 12.40805626191516353, 93.00000000000000000 ) ) ;
#5958 = CARTESIAN_POINT ( 'NONE',  ( -5.582510911615395699, 27.25430150734737111, -233.3200100877314469 ) ) ;
#5959 = CARTESIAN_POINT ( 'NONE',  ( -17.20794623181132721, 21.97849129791581291, -217.9187454682870850 ) ) ;
#5960 = CARTESIAN_POINT ( 'NONE',  ( -23.63383474287343589, -9.908731599815467916, -232.6396219513094081 ) ) ;
#5961 = CARTESIAN_POINT ( 'NONE',  ( -3.060450601941519189, 13.29454208326677289, -222.0135664617158682 ) ) ;
#5962 = CARTESIAN_POINT ( 'NONE',  ( -21.89065952084848021, -0.9940043559354364566, -216.9999999999999716 ) ) ;
#5963 = AXIS2_PLACEMENT_3D ( 'NONE', #21882, #19854, #7842 ) ;
#5964 = AXIS2_PLACEMENT_3D ( 'NONE', #10827, #2378, #7354 ) ;
#5965 = CARTESIAN_POINT ( 'NONE',  ( 15.50779141722566656, -5.694711448414747856, -219.6385356284298211 ) ) ;
#5966 = CARTESIAN_POINT ( 'NONE',  ( -5.590964611773372894, 13.92546790642523113, -228.7941110425196882 ) ) ;
#5967 = CARTESIAN_POINT ( 'NONE',  ( 29.64577750251057608, 2.839131411071813549, -220.9704389295326905 ) ) ;
#5968 = CARTESIAN_POINT ( 'NONE',  ( -21.93900267957129557, 7.862893636934532360, -233.4951761057262161 ) ) ;
#5969 = CARTESIAN_POINT ( 'NONE',  ( 14.68783945462866924, 9.535285537539673228, -219.4694094309942045 ) ) ;
#5970 = CARTESIAN_POINT ( 'NONE',  ( 0.000000000000000000, 0.000000000000000000, -74.48236190979496030 ) ) ;
#5971 = CARTESIAN_POINT ( 'NONE',  ( -6.702936938788568888, 25.88675107068059944, -218.1129661040884287 ) ) ;
#5972 = CARTESIAN_POINT ( 'NONE',  ( -21.63546480557098306, -21.44004028177477750, -223.8762611443524122 ) ) ;
#5973 = CARTESIAN_POINT ( 'NONE',  ( 17.43816562714825125, 15.15720016074785903, -232.3748236813696906 ) ) ;
#5974 = CARTESIAN_POINT ( 'NONE',  ( -7.475691298859681311, -12.42146568352542779, -226.9176918848390017 ) ) ;
#5975 = AXIS2_PLACEMENT_3D ( 'NONE', #12852, #16554, #20027 ) ;
#5976 = LINE ( 'NONE', #11383, #9937 ) ;
#5977 = CARTESIAN_POINT ( 'NONE',  ( -13.37045227479810094, 5.250293981428504786, -224.2914120185227205 ) ) ;
#5978 = CARTESIAN_POINT ( 'NONE',  ( 11.81564506561547390, -6.597897255275705142, -225.1493936678799628 ) ) ;
#5979 = EDGE_CURVE ( 'NONE', #15933, #10297, #7395, .T. ) ;
#5980 = CARTESIAN_POINT ( 'NONE',  ( 3.198229568054530070, 16.42319727383711481, -222.3960047798183552 ) ) ;
#5981 = CARTESIAN_POINT ( 'NONE',  ( -15.82622499106666325, 9.895986579907866343, -218.5115209877527604 ) ) ;
#5982 = CARTESIAN_POINT ( 'NONE',  ( -31.04415783139704388, 5.868882651865275690, -221.1472518903637194 ) ) ;
#5983 = CARTESIAN_POINT ( 'NONE',  ( -7.384981288797311194, -12.33405319921006615, -226.2189290763054998 ) ) ;
#5984 = APPLICATION_CONTEXT ( 'automotive_design' ) ;
#5985 = CARTESIAN_POINT ( 'NONE',  ( 18.03440114592047649, 4.755211820135348155, -216.3599228381250157 ) ) ;
#5986 = DIRECTION ( 'NONE',  ( 1.000000000000000000, 0.000000000000000000, -0.000000000000000000 ) ) ;
#5987 = CARTESIAN_POINT ( 'NONE',  ( -25.41475252190474521, -13.58614899836300260, -217.5872217295323310 ) ) ;
#5988 = CARTESIAN_POINT ( 'NONE',  ( 3.192353461299334061, 22.13718518159985393, -217.1103300728619843 ) ) ;
#5989 = CARTESIAN_POINT ( 'NONE',  ( 18.40125535140034430, 0.01434342441762339639, -233.2485400239426099 ) ) ;
#5990 = CARTESIAN_POINT ( 'NONE',  ( -5.562203253303141359, 12.75725363875033302, -225.3078268727488478 ) ) ;
#5991 = CARTESIAN_POINT ( 'NONE',  ( 14.28815361401014172, 13.86049093364188778, -216.0585456615740156 ) ) ;
#5992 = CARTESIAN_POINT ( 'NONE',  ( -1.243024450407066439, -19.42038079238686876, -231.9048276842376595 ) ) ;
#5993 = ORIENTED_EDGE ( 'NONE', *, *, #16056, .T. ) ;
#5994 = CARTESIAN_POINT ( 'NONE',  ( -7.084830653876206696, -25.45310193036084456, -219.3007580301989492 ) ) ;
#5995 = CARTESIAN_POINT ( 'NONE',  ( 24.03642272140365677, 3.646960756862087205, -218.2320643939070806 ) ) ;
#5996 = CARTESIAN_POINT ( 'NONE',  ( 19.88636028791461641, -20.85574262981397453, -219.9907771812986823 ) ) ;
#5997 = CARTESIAN_POINT ( 'NONE',  ( -22.53818779203657741, -7.663114047788936567, -232.6164956747681458 ) ) ;
#5998 = CARTESIAN_POINT ( 'NONE',  ( -11.40116373163465369, -15.95513543764466213, -216.7841692646331353 ) ) ;
#5999 = CARTESIAN_POINT ( 'NONE',  ( 11.39755372583812587, 20.40856199875060639, -231.2895618162029621 ) ) ;
#6000 = SURFACE_STYLE_FILL_AREA ( #4412 ) ;
#6001 = CARTESIAN_POINT ( 'NONE',  ( -12.10179538005628963, 1.685214252672075030, -222.4835512146784424 ) ) ;
#6002 = CARTESIAN_POINT ( 'NONE',  ( 3.763426558366607111, 28.60172112197566818, -230.1816715025297526 ) ) ;
#6003 = CARTESIAN_POINT ( 'NONE',  ( 3.635089269978064141, 27.05650967970794341, -222.4639105745756638 ) ) ;
#6004 = CARTESIAN_POINT ( 'NONE',  ( 23.46500920064399409, -11.67104692860896620, -233.8722294412333724 ) ) ;
#6005 = EDGE_LOOP ( 'NONE', ( #6256, #20651, #15858, #3909 ) ) ;
#6006 = CARTESIAN_POINT ( 'NONE',  ( 14.69853173970351179, 23.44775873627089524, -231.2711109634281001 ) ) ;
#6007 = CARTESIAN_POINT ( 'NONE',  ( -12.15411956849120756, 11.21601165624538687, -228.1895064089065670 ) ) ;
#6008 = CARTESIAN_POINT ( 'NONE',  ( -17.91550223652134122, 4.809113705933536487, -230.6324822114035555 ) ) ;
#6009 = CARTESIAN_POINT ( 'NONE',  ( -4.902442737337177725, -13.94343087703807704, -224.3742458082145959 ) ) ;
#6010 = CARTESIAN_POINT ( 'NONE',  ( 0.000000000000000000, 0.000000000000000000, 60.00000000000001421 ) ) ;
#6011 = CARTESIAN_POINT ( 'NONE',  ( 0.000000000000000000, 0.000000000000000000, 95.00000000000000000 ) ) ;
#6012 = CARTESIAN_POINT ( 'NONE',  ( 5.017623471397871349, 29.83561274492976878, -222.9769172135417250 ) ) ;
#6013 = CARTESIAN_POINT ( 'NONE',  ( 13.82101996411362244, -10.82539765916244789, -229.0162845096555770 ) ) ;
#6014 = DIRECTION ( 'NONE',  ( 0.000000000000000000, 0.000000000000000000, 1.000000000000000000 ) ) ;
#6015 = CARTESIAN_POINT ( 'NONE',  ( -11.28700884291539630, -21.85791790461604478, -233.5354093188319951 ) ) ;
#6016 =( NAMED_UNIT ( * ) SI_UNIT ( $, .STERADIAN. ) SOLID_ANGLE_UNIT ( ) );
#6017 = CARTESIAN_POINT ( 'NONE',  ( 5.017623471397871349, 29.83561274492976878, -222.9769172135417250 ) ) ;
#6018 = PRODUCT_DEFINITION ( 'UNKNOWN', '', #3461, #1320 ) ;
#6019 = CARTESIAN_POINT ( 'NONE',  ( -0.2269548806647709305, 12.31484924552052718, -228.6688778050056783 ) ) ;
#6020 = ORIENTED_EDGE ( 'NONE', *, *, #18896, .F. ) ;
#6021 = CARTESIAN_POINT ( 'NONE',  ( -11.98736441306973077, 11.45674391201457176, -217.8252237716743025 ) ) ;
#6022 = CARTESIAN_POINT ( 'NONE',  ( -26.76734473129764069, -3.453818734898710829, -232.3222361544058003 ) ) ;
#6023 = FACE_OUTER_BOUND ( 'NONE', #16405, .T. ) ;
#6024 = CARTESIAN_POINT ( 'NONE',  ( -22.24636130842955595, 5.845994931192185717, -8.119638057951140908 ) ) ;
#6025 = CARTESIAN_POINT ( 'NONE',  ( -7.913358619554302642, 16.16796202616373890, -233.0981776325470491 ) ) ;
#6026 = CARTESIAN_POINT ( 'NONE',  ( -14.99584720478923572, -27.01727836854440312, -219.7524089968786996 ) ) ;
#6027 = CARTESIAN_POINT ( 'NONE',  ( 13.28406271702445274, -5.237238614233280742, -225.2640488721434622 ) ) ;
#6028 = CARTESIAN_POINT ( 'NONE',  ( -16.65698539163286540, 11.03290537638306112, -233.6474915129378758 ) ) ;
#6029 = CARTESIAN_POINT ( 'NONE',  ( -25.59521542166570640, 7.637420400166985424, -216.4190921938142935 ) ) ;
#6030 = CARTESIAN_POINT ( 'NONE',  ( 0.07890756785233743464, 25.14108539708653822, -218.4152285319504756 ) ) ;
#6031 = CARTESIAN_POINT ( 'NONE',  ( 22.92944763917984830, -2.808047465753843770E-15, -75.00000000000000000 ) ) ;
#6032 = CARTESIAN_POINT ( 'NONE',  ( 14.18323607655884722, 3.286047475533308226, -222.8710065128477140 ) ) ;
#6033 = CARTESIAN_POINT ( 'NONE',  ( -12.46707500365009480, -15.03319212650626824, -230.3369784839848933 ) ) ;
#6034 = ORIENTED_EDGE ( 'NONE', *, *, #17641, .F. ) ;
#6035 = CARTESIAN_POINT ( 'NONE',  ( 5.833753951408669813, 12.47745132051510453, -226.2508980627489450 ) ) ;
#6036 = CARTESIAN_POINT ( 'NONE',  ( -12.70465517376339193, 12.03139199664008530, -229.6235454691090752 ) ) ;
#6037 = CARTESIAN_POINT ( 'NONE',  ( -21.72273972318264867, 21.08396222359856864, -224.0477214759881690 ) ) ;
#6038 = CARTESIAN_POINT ( 'NONE',  ( 30.39189047201120175, -1.943849802383817993, -228.0804048816970919 ) ) ;
#6039 = CARTESIAN_POINT ( 'NONE',  ( 25.50000000000000000, -0.5000000000000000000, 0.000000000000000000 ) ) ;
#6040 = ORIENTED_EDGE ( 'NONE', *, *, #20887, .F. ) ;
#6041 = CARTESIAN_POINT ( 'NONE',  ( -24.68906941503829700, 2.445024713909649705, -232.6803430500543755 ) ) ;
#6042 = CARTESIAN_POINT ( 'NONE',  ( -6.657868545208735611, -13.01156946085308874, -219.4730114480542227 ) ) ;
#6043 = CARTESIAN_POINT ( 'NONE',  ( 13.84082998555989974, 1.588769853554271361, -227.5469802220412134 ) ) ;
#6044 = CARTESIAN_POINT ( 'NONE',  ( 0.6364901924797052857, 13.89978473517355617, -221.8840706290426397 ) ) ;
#6045 = CARTESIAN_POINT ( 'NONE',  ( 25.50000000000000000, -0.5000000000000000000, 0.000000000000000000 ) ) ;
#6046 = CARTESIAN_POINT ( 'NONE',  ( -20.67624351032310059, -0.8683020119106035217, -219.0957770725675005 ) ) ;
#6047 = CARTESIAN_POINT ( 'NONE',  ( 10.39636392256998221, 18.46527700675686035, -215.1860221565626148 ) ) ;
#6048 = FILL_AREA_STYLE ('',( #13253 ) ) ;
#6049 = CARTESIAN_POINT ( 'NONE',  ( 14.05129436669267662, 0.2182301052511314010, -222.0076932542802695 ) ) ;
#6050 = CARTESIAN_POINT ( 'NONE',  ( 26.48990917286906921, 12.16675355942207659, -225.0153622588060216 ) ) ;
#6051 = CIRCLE ( 'NONE', #19700, 2.000000000000000000 ) ;
#6052 = DIRECTION ( 'NONE',  ( -1.000000000000000000, 0.000000000000000000, 0.000000000000000000 ) ) ;
#6053 = CARTESIAN_POINT ( 'NONE',  ( 16.72004689093256857, -4.507886829375356008, -228.6412576449023959 ) ) ;
#6054 = CARTESIAN_POINT ( 'NONE',  ( -23.54665576872953636, -14.78900941482413067, -230.7594827126482073 ) ) ;
#6055 = DIRECTION ( 'NONE',  ( 1.000000000000000000, 0.000000000000000000, 0.000000000000000000 ) ) ;
#6056 = DIRECTION ( 'NONE',  ( 1.000000000000000000, 0.000000000000000000, 0.000000000000000000 ) ) ;
#6057 = CARTESIAN_POINT ( 'NONE',  ( -1.248802714212398968, 14.93471382136348602, -228.4293827518713158 ) ) ;
#6058 = CARTESIAN_POINT ( 'NONE',  ( 13.95860357795928941, -2.197645239214564672, -231.3209047126647988 ) ) ;
#6059 = CARTESIAN_POINT ( 'NONE',  ( 13.62757736989142465, -5.584028114184929947, -227.2616851496390211 ) ) ;
#6060 = CARTESIAN_POINT ( 'NONE',  ( -14.58575946311604277, 2.190332613129932327, -228.6717927865686590 ) ) ;
#6061 = CARTESIAN_POINT ( 'NONE',  ( 16.69977105456987232, 16.51652889326612694, -233.6667933521891030 ) ) ;
#6062 = CARTESIAN_POINT ( 'NONE',  ( 14.66646255503707152, 18.43809875292740230, -219.3480462970252063 ) ) ;
#6063 = VERTEX_POINT ( 'NONE', #17742 ) ;
#6064 = CARTESIAN_POINT ( 'NONE',  ( 5.447232503735224718, -25.66160541809718865, -232.3984543420957323 ) ) ;
#6065 = DIRECTION ( 'NONE',  ( -1.000000000000000000, 0.000000000000000000, 0.000000000000000000 ) ) ;
#6066 = EDGE_CURVE ( 'NONE', #13719, #18650, #19408, .T. ) ;
#6067 = EDGE_CURVE ( 'NONE', #5788, #2867, #15536, .T. ) ;
#6068 = CARTESIAN_POINT ( 'NONE',  ( -13.31245686955614005, 26.96290519511623174, -230.1796856776773836 ) ) ;
#6069 = CARTESIAN_POINT ( 'NONE',  ( -9.747505956077446854, 15.39125695327449783, -233.2799778227147840 ) ) ;
#6070 = CARTESIAN_POINT ( 'NONE',  ( 24.55456120837795808, -10.86188008310946351, -220.0712554825904590 ) ) ;
#6071 = CARTESIAN_POINT ( 'NONE',  ( -6.474151797443945533, 21.29193859232740138, -215.9573456447696458 ) ) ;
#6072 = CARTESIAN_POINT ( 'NONE',  ( -25.00000000000000000, 0.000000000000000000, -75.00000000000000000 ) ) ;
#6073 = CARTESIAN_POINT ( 'NONE',  ( -0.1452471002967452851, 24.29564289358754081, -234.0861481044164805 ) ) ;
#6074 = CARTESIAN_POINT ( 'NONE',  ( 15.06072304412464291, 3.291435955319735651, -218.8606307204261725 ) ) ;
#6075 = CARTESIAN_POINT ( 'NONE',  ( -11.67631226053870996, 6.737291529340801333, -227.3110382950315227 ) ) ;
#6076 = CARTESIAN_POINT ( 'NONE',  ( 15.61962121506769385, 4.525360868525488911, -229.0684696061408090 ) ) ;
#6077 = CARTESIAN_POINT ( 'NONE',  ( 0.000000000000000000, 0.000000000000000000, -60.00000000000000000 ) ) ;
#6078 = CARTESIAN_POINT ( 'NONE',  ( 1.847452069095833593, 15.11597492720254543, -223.6261404253179421 ) ) ;
#6079 = CARTESIAN_POINT ( 'NONE',  ( -22.51170993270524789, -14.32174306031543054, -231.7292175355062795 ) ) ;
#6080 = CARTESIAN_POINT ( 'NONE',  ( 10.55627441269396094, 10.31758739525044888, -223.1990319438957613 ) ) ;
#6081 = CARTESIAN_POINT ( 'NONE',  ( -3.630465294598614889, -13.73165509241056093, -221.1424077787270619 ) ) ;
#6082 = CARTESIAN_POINT ( 'NONE',  ( 19.81538647100178707, 2.076704763782484253, -222.8269995749336658 ) ) ;
#6083 = CARTESIAN_POINT ( 'NONE',  ( -14.35594238341465889, 9.236863657925704629, -219.6542735655305307 ) ) ;
#6084 = CARTESIAN_POINT ( 'NONE',  ( 17.47229821656412341, -21.26691171910925249, -219.4940788861217413 ) ) ;
#6085 = CARTESIAN_POINT ( 'NONE',  ( 3.281983756374524663, 15.83593597903271721, -223.8697822987047346 ) ) ;
#6086 = CARTESIAN_POINT ( 'NONE',  ( -9.954421844142357756, 11.21484508112568079, -226.0177122452137439 ) ) ;
#6087 = CARTESIAN_POINT ( 'NONE',  ( -13.63292518690856170, 3.968236334994402981, -218.3158317831635316 ) ) ;
#6088 = CARTESIAN_POINT ( 'NONE',  ( -20.58881354142085485, -10.73024182470851606, -219.1570184730780397 ) ) ;
#6089 = EDGE_CURVE ( 'NONE', #11804, #758, #17648, .T. ) ;
#6090 = CARTESIAN_POINT ( 'NONE',  ( 13.21888801141564151, 2.135177519634172238, -228.0426311217386797 ) ) ;
#6091 = FACE_OUTER_BOUND ( 'NONE', #3051, .T. ) ;
#6092 = CARTESIAN_POINT ( 'NONE',  ( -9.690988788510356500, -7.266623515821958534, -222.7221403394456445 ) ) ;
#6093 = CARTESIAN_POINT ( 'NONE',  ( -1.975202609796049336, 20.81351768191813889, -217.5779402428482001 ) ) ;
#6094 = CARTESIAN_POINT ( 'NONE',  ( 24.19635128940818447, 10.31396593861802380, -216.9479509989864425 ) ) ;
#6095 = CARTESIAN_POINT ( 'NONE',  ( -14.46024998630872282, 14.54669730493860946, -231.4156670963686508 ) ) ;
#6096 = ADVANCED_FACE ( 'NONE', ( #8051 ), #16161, .T. ) ;
#6097 = CARTESIAN_POINT ( 'NONE',  ( 12.92410717862594893, 29.37236178718849189, -224.5435071569520744 ) ) ;
#6098 = ORIENTED_EDGE ( 'NONE', *, *, #13277, .T. ) ;
#6099 = CARTESIAN_POINT ( 'NONE',  ( 0.8935217740153370558, -25.09083646304939919, -218.5222943608621335 ) ) ;
#6100 = ORIENTED_EDGE ( 'NONE', *, *, #22062, .F. ) ;
#6101 = CARTESIAN_POINT ( 'NONE',  ( -1.827935560680505445, -14.81092009092713369, -225.7372845858837707 ) ) ;
#6102 = CARTESIAN_POINT ( 'NONE',  ( 23.49048926389013658, 9.645778135078892035, -218.7307869890797463 ) ) ;
#6103 = CARTESIAN_POINT ( 'NONE',  ( 13.62757736989142465, -5.584028114184929947, -227.2616851496390211 ) ) ;
#6104 = ADVANCED_FACE ( 'NONE', ( #12781 ), #21530, .T. ) ;
#6105 = CARTESIAN_POINT ( 'NONE',  ( 24.67321061357916889, 1.914345543126667826, -232.4367140101115581 ) ) ;
#6106 = CARTESIAN_POINT ( 'NONE',  ( -15.46269062504165781, -26.67469327287815517, -225.2085449711190677 ) ) ;
#6107 = CARTESIAN_POINT ( 'NONE',  ( 10.64798096806036121, 19.48085866535796740, -231.3996658690317361 ) ) ;
#6108 = DIRECTION ( 'NONE',  ( 0.000000000000000000, 0.000000000000000000, 1.000000000000000000 ) ) ;
#6109 = CARTESIAN_POINT ( 'NONE',  ( 15.80790828609669951, 3.698719088746416972, -219.8106174092292804 ) ) ;
#6110 = CARTESIAN_POINT ( 'NONE',  ( 5.069241901512100412, 14.34986542013820632, -229.6420000777802954 ) ) ;
#6111 = CARTESIAN_POINT ( 'NONE',  ( 9.382249691333727881, 26.55946126407900820, -224.4468135941759215 ) ) ;
#6112 = CARTESIAN_POINT ( 'NONE',  ( 14.87770435525805013, -9.987123395515542512, -215.8225415630120665 ) ) ;
#6113 = CARTESIAN_POINT ( 'NONE',  ( 22.20554449732931346, 18.01468431515759860, -218.9348803756412849 ) ) ;
#6114 = CARTESIAN_POINT ( 'NONE',  ( -15.19607346356906952, 9.485739149828241068, -229.2407115334993080 ) ) ;
#6115 = CARTESIAN_POINT ( 'NONE',  ( -15.54392142943450317, 6.670312097614393920, -219.6934017696036676 ) ) ;
#6116 = CARTESIAN_POINT ( 'NONE',  ( -5.429593058350183910, -25.95961553913046416, -230.5291520159703111 ) ) ;
#6117 = CARTESIAN_POINT ( 'NONE',  ( 1.232595164407830946E-29, -17.50000000000007105, -24.99999999999999645 ) ) ;
#6118 = CARTESIAN_POINT ( 'NONE',  ( 16.38151749656409351, 8.902090001712490874, -231.2955017965201989 ) ) ;
#6119 = CARTESIAN_POINT ( 'NONE',  ( 20.36520141328406552, -18.94542628267938156, -227.6082859645964902 ) ) ;
#6120 = CARTESIAN_POINT ( 'NONE',  ( 26.00000000000000000, 4.399999999999999467, -3.300000000000000266 ) ) ;
#6121 = CLOSED_SHELL ( 'NONE', ( #12847, #3315, #16155, #14625, #10429, #11066, #5412, #675, #13179, #7851, #4563, #9537, #4454, #11996, #15745, #20265, #9697, #5122, #8869, #6391, #11293, #2499, #19277, #18487, #15624, #16025, #1554, #19487, #1444, #20603, #18040, #4915, #9784, #11829, #20161, #12040, #9089, #18646, #787, #10106, #9424, #9813, #3772, #12158 ) ) ;
#6122 = CARTESIAN_POINT ( 'NONE',  ( -5.804961988600464196, -12.67915086496026511, -228.7923277404792088 ) ) ;
#6123 = APPLICATION_PROTOCOL_DEFINITION ( 'draft international standard', 'automotive_design', 1998, #5686 ) ;
#6124 = CARTESIAN_POINT ( 'NONE',  ( 5.069241901512100412, 14.34986542013820632, -229.6420000777802954 ) ) ;
#6125 = CARTESIAN_POINT ( 'NONE',  ( -4.155456637169709921, 11.30291311430030987, -225.2606024264729001 ) ) ;
#6126 = VERTEX_POINT ( 'NONE', #9731 ) ;
#6127 = CARTESIAN_POINT ( 'NONE',  ( -19.00318367631585659, 13.14621133775862916, -233.8403879275295765 ) ) ;
#6128 = CARTESIAN_POINT ( 'NONE',  ( 24.22993967103762714, -2.502297861120115208, -232.9814837474525007 ) ) ;
#6129 = CARTESIAN_POINT ( 'NONE',  ( 21.96352831578809273, -0.3315607655629317918, -233.9427286327412503 ) ) ;
#6130 = CARTESIAN_POINT ( 'NONE',  ( -22.00000000000001421, 0.000000000000000000, -224.9999999999999716 ) ) ;
#6131 = CARTESIAN_POINT ( 'NONE',  ( -6.855867220396999251, 12.17758473459128332, -220.6375607554995213 ) ) ;
#6132 = CARTESIAN_POINT ( 'NONE',  ( -9.794218246645117532, -15.26311849320921255, -215.4893187949746505 ) ) ;
#6133 = CARTESIAN_POINT ( 'NONE',  ( 14.02668320743028119, -5.282748560960272677, -221.9001732195871739 ) ) ;
#6134 = SHAPE_REPRESENTATION ( 'shaft', ( #6677 ), #8503 ) ;
#6135 = CARTESIAN_POINT ( 'NONE',  ( -23.52999999174766543, 19.39566142560855866, -221.9446938626390704 ) ) ;
#6136 = CARTESIAN_POINT ( 'NONE',  ( -20.49711526797010208, 7.006997077916217620, -215.3369776077118445 ) ) ;
#6137 = ORIENTED_EDGE ( 'NONE', *, *, #7781, .T. ) ;
#6138 = CARTESIAN_POINT ( 'NONE',  ( -1.837924626891132229, 29.27703531260187475, -227.2344808100871774 ) ) ;
#6139 = DIRECTION ( 'NONE',  ( 1.000000000000000000, 0.000000000000000000, 0.000000000000000000 ) ) ;
#6140 = CARTESIAN_POINT ( 'NONE',  ( -14.37318171526297483, 2.227741863946853140, -231.7654527934561202 ) ) ;
#6141 = CARTESIAN_POINT ( 'NONE',  ( -12.44689724543316522, -19.26441470091720731, -219.1960634559673622 ) ) ;
#6142 = ORIENTED_EDGE ( 'NONE', *, *, #6089, .F. ) ;
#6143 = CARTESIAN_POINT ( 'NONE',  ( -17.78731991475362406, 16.78509880370027929, -218.2387321183659310 ) ) ;
#6144 = CARTESIAN_POINT ( 'NONE',  ( 10.12956299421491302, 11.38773431477224385, -230.3175791991728829 ) ) ;
#6145 = CARTESIAN_POINT ( 'NONE',  ( 3.711349367426693746, 16.84755988915346236, -233.7359972593521888 ) ) ;
#6146 = CARTESIAN_POINT ( 'NONE',  ( -14.26213125333782727, -4.747741064748048245, -225.2154851558723294 ) ) ;
#6147 = LINE ( 'NONE', #5930, #15424 ) ;
#6148 = ORIENTED_EDGE ( 'NONE', *, *, #17705, .F. ) ;
#6149 = CARTESIAN_POINT ( 'NONE',  ( -11.49049084071896409, 11.06834963248926940, -218.3354249205727058 ) ) ;
#6150 = CARTESIAN_POINT ( 'NONE',  ( -8.875208054371373834, -23.27682998066124398, -233.1222812539844540 ) ) ;
#6151 = CARTESIAN_POINT ( 'NONE',  ( 25.18785298611088308, 3.974282393449815931, -218.7636041058819956 ) ) ;
#6152 = CARTESIAN_POINT ( 'NONE',  ( -3.003186468682855104, 15.63968344752823469, -231.5301608670590667 ) ) ;
#6153 = DIRECTION ( 'NONE',  ( 0.000000000000000000, 0.000000000000000000, 1.000000000000000000 ) ) ;
#6154 = CARTESIAN_POINT ( 'NONE',  ( -18.04102731735134313, 0.8647102676311391178, -229.4625228093430849 ) ) ;
#6155 = CARTESIAN_POINT ( 'NONE',  ( 11.00045714400293306, 20.20239058357963913, -215.1666500215986275 ) ) ;
#6156 = CARTESIAN_POINT ( 'NONE',  ( -24.96693800283771836, 1.326846381236610473, -9.917101879163732647 ) ) ;
#6157 = CARTESIAN_POINT ( 'NONE',  ( 23.49048926389013658, 9.645778135078892035, -218.7307869890797463 ) ) ;
#6158 = DIRECTION ( 'NONE',  ( -0.000000000000000000, 0.000000000000000000, -1.000000000000000000 ) ) ;
#6159 = CARTESIAN_POINT ( 'NONE',  ( 27.03411061974195562, -3.460823241630351710, -221.7771387205989413 ) ) ;
#6160 = CARTESIAN_POINT ( 'NONE',  ( -14.78079095050690661, -5.416970230978240153, -229.7193632018645246 ) ) ;
#6161 = DIRECTION ( 'NONE',  ( -0.000000000000000000, 0.000000000000000000, -1.000000000000000000 ) ) ;
#6162 = AXIS2_PLACEMENT_3D ( 'NONE', #3069, #18507, #11196 ) ;
#6163 = DIRECTION ( 'NONE',  ( -0.000000000000000000, 0.000000000000000000, -1.000000000000000000 ) ) ;
#6164 = CARTESIAN_POINT ( 'NONE',  ( -14.84124724799726991, 21.42277200659090042, -233.6300684249849553 ) ) ;
#6165 = CARTESIAN_POINT ( 'NONE',  ( 19.66172111867919270, -11.21951684559458506, -235.3531537740016972 ) ) ;
#6166 = CARTESIAN_POINT ( 'NONE',  ( 25.83609367470520723, -15.13481494965009411, -225.4685613576401124 ) ) ;
#6167 = CARTESIAN_POINT ( 'NONE',  ( -15.30295614572244922, 9.661125001905515930, -218.8475896279880146 ) ) ;
#6168 = CARTESIAN_POINT ( 'NONE',  ( 30.52813181070726856, 5.438803974502569361, -223.5441926215666513 ) ) ;
#6169 = CARTESIAN_POINT ( 'NONE',  ( 8.312165662451315384, 13.84431584962456974, -225.8109542921768025 ) ) ;
#6170 = VERTEX_POINT ( 'NONE', #19736 ) ;
#6171 = CARTESIAN_POINT ( 'NONE',  ( 3.520698644836853131, -14.14291361662535884, -221.2714412251625618 ) ) ;
#6172 = DIRECTION ( 'NONE',  ( 0.000000000000000000, 0.000000000000000000, 1.000000000000000000 ) ) ;
#6173 = CARTESIAN_POINT ( 'NONE',  ( -16.85225081326727903, 6.237400186851330020, -234.5847093771173206 ) ) ;
#6174 = AXIS2_PLACEMENT_3D ( 'NONE', #8047, #2845, #21863 ) ;
#6175 = CARTESIAN_POINT ( 'NONE',  ( -4.296082356836364191, 12.57880442405704002, -229.5247240216588125 ) ) ;
#6176 = CARTESIAN_POINT ( 'NONE',  ( 3.490829917597003895, 11.40812925993816229, -222.8973702487053004 ) ) ;
#6177 = CARTESIAN_POINT ( 'NONE',  ( 15.40548389857710987, -8.435137368586953954, -220.3367290259554920 ) ) ;
#6178 = CARTESIAN_POINT ( 'NONE',  ( -9.740348021262962064, 16.12529029871877384, -216.4361617420699702 ) ) ;
#6179 = CARTESIAN_POINT ( 'NONE',  ( 10.07835692657692128, -10.42743089613093233, 93.00000000000002842 ) ) ;
#6180 = ADVANCED_FACE ( 'NONE', ( #4544, #18180 ), #1176, .F. ) ;
#6181 = AXIS2_PLACEMENT_3D ( 'NONE', #14396, #5369, #21015 ) ;
#6182 = CARTESIAN_POINT ( 'NONE',  ( -2.328291070394212792, 14.80737693666302945, -219.0291440940735868 ) ) ;
#6183 = CARTESIAN_POINT ( 'NONE',  ( 30.57915561709945251, 3.468229287067555067, -223.8876084027091906 ) ) ;
#6184 = CARTESIAN_POINT ( 'NONE',  ( -24.02434186778878455, 18.57431834865475651, -228.2662945587547370 ) ) ;
#6185 = CARTESIAN_POINT ( 'NONE',  ( 15.76910524310159900, 5.601482066865847820, -220.3440822020379528 ) ) ;
#6186 = CARTESIAN_POINT ( 'NONE',  ( 6.608541902967795423, 16.43938546752961116, -220.2982508316308952 ) ) ;
#6187 = DIRECTION ( 'NONE',  ( -0.000000000000000000, -0.000000000000000000, 1.000000000000000000 ) ) ;
#6188 = CARTESIAN_POINT ( 'NONE',  ( 9.132190541728901323, 17.73033835127231939, -219.5524510795130766 ) ) ;
#6189 = CARTESIAN_POINT ( 'NONE',  ( -18.89430729770302975, -12.42271633246521212, -233.2230176520695295 ) ) ;
#6190 = CARTESIAN_POINT ( 'NONE',  ( 22.84140515590350518, 18.29101041979067332, -226.2334522600520472 ) ) ;
#6191 = CARTESIAN_POINT ( 'NONE',  ( -1.232290808404003624, -30.06229647885771428, -229.8325228448912583 ) ) ;
#6192 = TOROIDAL_SURFACE ( 'NONE', #10878, 22.63401512838748175, 3.000000000000002665 ) ;
#6193 = CARTESIAN_POINT ( 'NONE',  ( -23.92685091328690916, 2.930194138463273749E-15, 80.43141006107198621 ) ) ;
#6194 = CIRCLE ( 'NONE', #10881, 2.000000000000000000 ) ;
#6195 = CARTESIAN_POINT ( 'NONE',  ( -11.08731210905863840, 25.61052584666692766, -228.9953606804266997 ) ) ;
#6196 =( NAMED_UNIT ( * ) PLANE_ANGLE_UNIT ( ) SI_UNIT ( $, .RADIAN. ) );
#6197 = CARTESIAN_POINT ( 'NONE',  ( 12.90505172109588194, -11.18139282378177768, -218.7382941517081747 ) ) ;
#6198 = CARTESIAN_POINT ( 'NONE',  ( 26.39436175479395885, 14.32821500273865034, -221.6819523832376149 ) ) ;
#6199 = CARTESIAN_POINT ( 'NONE',  ( -20.97727766418175932, 9.381545086430262970, -232.5968905491617420 ) ) ;
#6200 = CARTESIAN_POINT ( 'NONE',  ( -12.38801939673351704, 9.361418580567464787, -232.8075769614211765 ) ) ;
#6201 = CARTESIAN_POINT ( 'NONE',  ( -16.42300678490213883, -6.478264502461970054, -228.9348778629521064 ) ) ;
#6202 = CARTESIAN_POINT ( 'NONE',  ( 10.93653298376230687, 10.42959444671468106, -232.5920418140667039 ) ) ;
#6203 = CARTESIAN_POINT ( 'NONE',  ( 17.50000000000001066, 0.000000000000000000, -55.00000000000000711 ) ) ;
#6204 = CARTESIAN_POINT ( 'NONE',  ( -14.71809293534535534, -5.923356948231951691, -217.5005292165803041 ) ) ;
#6205 = CARTESIAN_POINT ( 'NONE',  ( 7.213476267053916757, 16.78447451494783138, -217.5857052077849687 ) ) ;
#6206 = VECTOR ( 'NONE', #1708, 1000.000000000000000 ) ;
#6207 = CARTESIAN_POINT ( 'NONE',  ( -20.86570240061152148, 1.122719768445835875, -219.0984131021933763 ) ) ;
#6208 = AXIS2_PLACEMENT_3D ( 'NONE', #16866, #16639, #12105 ) ;
#6209 = CARTESIAN_POINT ( 'NONE',  ( -18.02718827071834085, 20.33515877052379395, -229.5060669840136143 ) ) ;
#6210 = CARTESIAN_POINT ( 'NONE',  ( 10.81638188557560731, 14.98959006186633403, -234.2424515599453514 ) ) ;
#6211 = EDGE_CURVE ( 'NONE', #2867, #3431, #3966, .T. ) ;
#6212 = VERTEX_POINT ( 'NONE', #6120 ) ;
#6213 = CARTESIAN_POINT ( 'NONE',  ( 3.499756879752360827, -15.16424639601953039, -225.9472731234413061 ) ) ;
#6214 = CARTESIAN_POINT ( 'NONE',  ( 1.967796959512672306, -15.42100964229427085, -222.1538042820122314 ) ) ;
#6215 = CARTESIAN_POINT ( 'NONE',  ( -24.77996431573922820, 10.49354383977773786, -234.1655613096203581 ) ) ;
#6216 = CARTESIAN_POINT ( 'NONE',  ( 14.02668320743028119, -5.282748560960272677, -221.9001732195871739 ) ) ;
#6217 = CARTESIAN_POINT ( 'NONE',  ( -18.11268275035277853, -3.459088653808292335, -218.4233329573673359 ) ) ;
#6218 = CARTESIAN_POINT ( 'NONE',  ( -21.52428768452188734, -21.65989873160339840, -225.4304055049964006 ) ) ;
#6219 = CARTESIAN_POINT ( 'NONE',  ( 3.689800395305025127, 23.07294874520714956, -219.2515233573129478 ) ) ;
#6220 = DIRECTION ( 'NONE',  ( 0.000000000000000000, 0.000000000000000000, -1.000000000000000000 ) ) ;
#6221 = CARTESIAN_POINT ( 'NONE',  ( -17.17981675979428147, 1.478343374046288128, -216.2419730925687418 ) ) ;
#6222 = CARTESIAN_POINT ( 'NONE',  ( 4.340445191644851874, 29.86837761166362881, -227.4879512554873315 ) ) ;
#6223 = CARTESIAN_POINT ( 'NONE',  ( 13.41709597927210496, 19.57823531746157997, -218.2666972400567147 ) ) ;
#6224 = CARTESIAN_POINT ( 'NONE',  ( 15.50373320885645079, -27.90820408561472732, -228.0623419774833280 ) ) ;
#6225 = AXIS2_PLACEMENT_3D ( 'NONE', #11498, #16348, #19926 ) ;
#6226 = AXIS2_PLACEMENT_3D ( 'NONE', #4579, #6381, #11234 ) ;
#6227 = CARTESIAN_POINT ( 'NONE',  ( 16.10596270516584028, 24.75152718569329835, -228.9330127594856492 ) ) ;
#6228 = CARTESIAN_POINT ( 'NONE',  ( -21.01242583983345469, 16.60754347445175227, -220.8286358486543293 ) ) ;
#6229 = CARTESIAN_POINT ( 'NONE',  ( -24.49083850720273148, 4.222094140707651100, -219.1543001448025905 ) ) ;
#6230 = ADVANCED_FACE ( 'NONE', ( #7830 ), #12616, .F. ) ;
#6231 = CARTESIAN_POINT ( 'NONE',  ( 5.920190106170357680, -27.41802839654005197, -221.0732524667164114 ) ) ;
#6232 = DIRECTION ( 'NONE',  ( -1.000000000000000000, 0.000000000000000000, 0.000000000000000000 ) ) ;
#6233 = DIRECTION ( 'NONE',  ( 1.000000000000000000, 0.000000000000000000, 0.000000000000000000 ) ) ;
#6234 = CARTESIAN_POINT ( 'NONE',  ( 20.41153371889344825, 17.18812948447019551, -230.7531656956970778 ) ) ;
#6235 = CARTESIAN_POINT ( 'NONE',  ( 14.94445598564424493, -12.06760924077967090, -230.4366326412025785 ) ) ;
#6236 = CARTESIAN_POINT ( 'NONE',  ( -28.61025869263052712, 6.891613135096296361, -222.2489362813765013 ) ) ;
#6237 = CARTESIAN_POINT ( 'NONE',  ( -7.531388159411753769, -21.98719092781708540, -216.0713624712111312 ) ) ;
#6238 = DIRECTION ( 'NONE',  ( 0.000000000000000000, 0.000000000000000000, 1.000000000000000000 ) ) ;
#6239 = CARTESIAN_POINT ( 'NONE',  ( 4.543450689403089271, 15.91052110650461771, -218.9437823786444426 ) ) ;
#6241 = CARTESIAN_POINT ( 'NONE',  ( 0.9169988354999972779, 20.59043933275470550, -235.2854195559275752 ) ) ;
#6240 = CIRCLE ( 'NONE', #9120, 2.000000000000000000 ) ;
#6242 = EDGE_LOOP ( 'NONE', ( #6509, #8810, #22156, #16186 ) ) ;
#6243 = CARTESIAN_POINT ( 'NONE',  ( -3.643097910890548796, 22.16888955197135047, -233.9701981029593298 ) ) ;
#6244 = CARTESIAN_POINT ( 'NONE',  ( -13.36955836198420577, -3.222265253903016990, -227.4060678739157026 ) ) ;
#6245 = CARTESIAN_POINT ( 'NONE',  ( -21.80000000000000071, 2.669730022141230095E-15, -78.50000000000000000 ) ) ;
#6246 = DIRECTION ( 'NONE',  ( -2.891205793294678696E-17, 0.000000000000000000, -1.000000000000000000 ) ) ;
#6247 = CARTESIAN_POINT ( 'NONE',  ( -17.39699619235753048, 15.64332637722790054, -216.0406373264262641 ) ) ;
#6248 = CARTESIAN_POINT ( 'NONE',  ( -9.037518995728490268, -13.81466884781966620, -216.3195389756191673 ) ) ;
#6249 = CARTESIAN_POINT ( 'NONE',  ( 25.83609367470520723, -15.13481494965009411, -225.4685613576401124 ) ) ;
#6250 = CARTESIAN_POINT ( 'NONE',  ( -2.958555384449997661, 13.07587799061801093, -222.7767538261418565 ) ) ;
#6251 = CARTESIAN_POINT ( 'NONE',  ( -27.05172747931452903, 14.36075930490012276, -228.5082213655825853 ) ) ;
#6252 = CARTESIAN_POINT ( 'NONE',  ( -9.290933312444883185, 29.15551353946876745, -225.8551562993724247 ) ) ;
#6253 = CARTESIAN_POINT ( 'NONE',  ( -14.87984907657228639, 0.2138881189739126887, -228.7773920408832282 ) ) ;
#6254 = CARTESIAN_POINT ( 'NONE',  ( 15.70179827786738969, 6.572001003133339125, -229.5476218741844434 ) ) ;
#6255 = CARTESIAN_POINT ( 'NONE',  ( -8.783466540727490113, -25.47690852953548557, -220.9562114332719318 ) ) ;
#6256 = ORIENTED_EDGE ( 'NONE', *, *, #11758, .F. ) ;
#6257 = CARTESIAN_POINT ( 'NONE',  ( -9.988594796049140356, 11.34066464990972811, -226.6453149279956563 ) ) ;
#6258 = CARTESIAN_POINT ( 'NONE',  ( 17.97920459523930958, 17.43922474653955490, -233.2737719749805763 ) ) ;
#6259 = CARTESIAN_POINT ( 'NONE',  ( 1.220475224794998370, 29.83033731899746144, -230.4224274340063801 ) ) ;
#6260 = ADVANCED_FACE ( 'NONE', ( #7607, #9625 ), #21757, .T. ) ;
#6261 = CARTESIAN_POINT ( 'NONE',  ( 13.66858788651615164, -3.112492835348085407, -221.5154270223497690 ) ) ;
#6262 = PLANE ( 'NONE',  #679 ) ;
#6263 = ORIENTED_EDGE ( 'NONE', *, *, #5142, .T. ) ;
#6264 = CARTESIAN_POINT ( 'NONE',  ( -9.250876228778270871, 9.538614635316015722, -227.1332118982684563 ) ) ;
#6265 = CARTESIAN_POINT ( 'NONE',  ( -6.443428446094314310, -19.32516562084312994, -233.2789765400915201 ) ) ;
#6266 = CARTESIAN_POINT ( 'NONE',  ( 14.98418162551161714, 4.450317369940187895, -227.9894155827521161 ) ) ;
#6267 = CIRCLE ( 'NONE', #14209, 2.000000000000000000 ) ;
#6268 = CARTESIAN_POINT ( 'NONE',  ( 12.53674998645855787, 17.96979015029927851, -232.8843215672231679 ) ) ;
#6269 = FACE_BOUND ( 'NONE', #11468, .T. ) ;
#6270 = CARTESIAN_POINT ( 'NONE',  ( -11.10182655035041144, 8.778638955377752850, -227.1050196202568827 ) ) ;
#6271 = CARTESIAN_POINT ( 'NONE',  ( 17.10545320562996352, 22.53742678899184781, -232.4605876935045785 ) ) ;
#6272 =( NAMED_UNIT ( * ) SI_UNIT ( $, .STERADIAN. ) SOLID_ANGLE_UNIT ( ) );
#6273 = CARTESIAN_POINT ( 'NONE',  ( -25.00000000000000000, 0.000000000000000000, -75.00000000000000000 ) ) ;
#6274 = CARTESIAN_POINT ( 'NONE',  ( 17.19674704922021391, 23.07334190050143974, -228.8256488842130238 ) ) ;
#6275 = FACE_OUTER_BOUND ( 'NONE', #21422, .T. ) ;
#6276 = CARTESIAN_POINT ( 'NONE',  ( 15.57890332219703389, -7.739300371747003027, -228.5080386124398899 ) ) ;
#6277 = CARTESIAN_POINT ( 'NONE',  ( -25.82802808205240552, -14.78441951539553401, -222.6940535085979604 ) ) ;
#6278 = CARTESIAN_POINT ( 'NONE',  ( -21.73688349724618263, -7.520329038248549480, -6.599172142090282911 ) ) ;
#6279 = AXIS2_PLACEMENT_3D ( 'NONE', #3029, #18689, #13394 ) ;
#6280 = DIRECTION ( 'NONE',  ( -1.000000000000000000, 0.000000000000000000, 0.000000000000000000 ) ) ;
#6281 = CARTESIAN_POINT ( 'NONE',  ( -0.4548635697939061306, 27.30478022265488036, -219.8474162243132071 ) ) ;
#6282 = CARTESIAN_POINT ( 'NONE',  ( 30.72375212156453372, -9.269427080566114086, -227.3728682798597731 ) ) ;
#6283 = CARTESIAN_POINT ( 'NONE',  ( 18.55298002304457228, -12.22359628793950570, -216.9137843736221782 ) ) ;
#6284 = CARTESIAN_POINT ( 'NONE',  ( -23.20103936322198024, 10.64725167743880085, -231.7714206262400864 ) ) ;
#6285 = CARTESIAN_POINT ( 'NONE',  ( -20.86570240061152148, 1.122719768445835875, -219.0984131021933763 ) ) ;
#6286 = CARTESIAN_POINT ( 'NONE',  ( 11.87550186346493497, 14.27797038184677270, -220.2068243228838185 ) ) ;
#6287 = ORIENTED_EDGE ( 'NONE', *, *, #17683, .F. ) ;
#6288 = CARTESIAN_POINT ( 'NONE',  ( -0.6326494355537284342, -15.87741594504987219, -229.6822519216137266 ) ) ;
#6289 = CARTESIAN_POINT ( 'NONE',  ( -10.20851360429410981, 10.29801091644274180, 92.99999999999998579 ) ) ;
#6290 = CARTESIAN_POINT ( 'NONE',  ( -30.17036082276531772, 5.959165309317525860, -219.4883053239162791 ) ) ;
#6291 = CARTESIAN_POINT ( 'NONE',  ( 18.69149182921226782, 24.00661454656289706, -229.8257469855424517 ) ) ;
#6292 = CARTESIAN_POINT ( 'NONE',  ( 4.401501667365108617, 18.53594119471695123, -215.1186850315663150 ) ) ;
#6293 = CARTESIAN_POINT ( 'NONE',  ( 13.21219219391003818, -8.064832675337259005, -225.0434479037668041 ) ) ;
#6294 = CARTESIAN_POINT ( 'NONE',  ( -6.571166997218196748, 12.74865329367398736, -229.9840124400968762 ) ) ;
#6295 = CARTESIAN_POINT ( 'NONE',  ( -14.10849459794400751, -0.2436790717799666162, -223.1085195285415921 ) ) ;
#6296 = AXIS2_PLACEMENT_3D ( 'NONE', #11354, #6055, #13153 ) ;
#6297 = CARTESIAN_POINT ( 'NONE',  ( 12.58033168766476528, 20.35631482982274676, -235.1670639654690547 ) ) ;
#6298 = CIRCLE ( 'NONE', #16361, 3.000000000000002665 ) ;
#6299 = CARTESIAN_POINT ( 'NONE',  ( -27.11599398522282911, 10.60460483532474996, -224.7310548435675912 ) ) ;
#6300 = CARTESIAN_POINT ( 'NONE',  ( -23.49379658590067876, 11.46840048879614393, -217.2519070826072323 ) ) ;
#6301 = CARTESIAN_POINT ( 'NONE',  ( 17.43816562714825125, 15.15720016074785903, -232.3748236813696906 ) ) ;
#6302 = CARTESIAN_POINT ( 'NONE',  ( 9.425340689562565544, 25.38932416188112384, -221.3391712389563963 ) ) ;
#6303 = FACE_OUTER_BOUND ( 'NONE', #5819, .T. ) ;
#6304 = CARTESIAN_POINT ( 'NONE',  ( 0.000000000000000000, 0.000000000000000000, 77.51594804401857175 ) ) ;
#6305 = CARTESIAN_POINT ( 'NONE',  ( 15.70200226922815290, 22.14006925444000018, -227.8255507828836244 ) ) ;
#6306 = CARTESIAN_POINT ( 'NONE',  ( -11.88525712185471050, -8.925198460467992589, -221.0951487055306472 ) ) ;
#6307 = CARTESIAN_POINT ( 'NONE',  ( 15.33737796850231305, 13.57479350230705428, -232.3313557812109025 ) ) ;
#6308 = CARTESIAN_POINT ( 'NONE',  ( -9.979217823323752512, -26.65442139683551659, -219.8174849573283325 ) ) ;
#6309 = DIRECTION ( 'NONE',  ( 0.000000000000000000, 0.000000000000000000, 1.000000000000000000 ) ) ;
#6310 = CARTESIAN_POINT ( 'NONE',  ( -4.386767007475907754, 14.39570986262862107, -223.2690175027443615 ) ) ;
#6311 = EDGE_CURVE ( 'NONE', #11616, #9103, #2482, .T. ) ;
#6312 = CARTESIAN_POINT ( 'NONE',  ( 24.05238142633148968, -17.07083877791421500, -221.4615098029387070 ) ) ;
#6313 = CARTESIAN_POINT ( 'NONE',  ( 17.98704291748025952, 16.14142602298251461, -217.3684083235702644 ) ) ;
#6314 = CARTESIAN_POINT ( 'NONE',  ( -5.365396334125453137, 16.47374957271378904, -219.4721119688156534 ) ) ;
#6315 = CARTESIAN_POINT ( 'NONE',  ( -20.73319232323294514, 5.144688277016327582, -214.6391322078443977 ) ) ;
#6316 = CARTESIAN_POINT ( 'NONE',  ( -17.33275459786259276, -4.423804729537573088, -220.8440611986277418 ) ) ;
#6317 = CARTESIAN_POINT ( 'NONE',  ( -27.32994399549947673, 3.379920396491164603, -227.9326384921875217 ) ) ;
#6318 = FACE_OUTER_BOUND ( 'NONE', #16511, .T. ) ;
#6319 = CARTESIAN_POINT ( 'NONE',  ( -29.62561404221338890, 0.9211338879504321620, -221.2478075149841743 ) ) ;
#6320 = CARTESIAN_POINT ( 'NONE',  ( 19.40629804599390340, 15.10110417999774057, -216.3942729496570223 ) ) ;
#6321 = CARTESIAN_POINT ( 'NONE',  ( 29.11492790716816614, 6.132849117128307270, -229.8316941169402412 ) ) ;
#6322 = CARTESIAN_POINT ( 'NONE',  ( -4.651113456395510326, 27.58151660986499110, -218.3072938287727141 ) ) ;
#6323 = CARTESIAN_POINT ( 'NONE',  ( 8.730612144237051453, 13.93563980088501886, -217.1627566045470132 ) ) ;
#6324 = COLOUR_RGB ( '', 0.09019608, 0.27058824, 0.51372549) ;
#6325 = ORIENTED_EDGE ( 'NONE', *, *, #15901, .F. ) ;
#6326 = CARTESIAN_POINT ( 'NONE',  ( 8.343784211782431015, -26.96289276196324636, -225.6651636531778422 ) ) ;
#6327 = ORIENTED_EDGE ( 'NONE', *, *, #11715, .T. ) ;
#6328 = CARTESIAN_POINT ( 'NONE',  ( 2.179383121900682951, -16.00498718933496889, -221.0566978482307832 ) ) ;
#6329 = CARTESIAN_POINT ( 'NONE',  ( -12.02603758797190459, 8.152912069735307909, -218.2257190893353709 ) ) ;
#6330 = CARTESIAN_POINT ( 'NONE',  ( 8.785770181087007913, -10.38731345016515917, -223.4272116603623317 ) ) ;
#6331 = CARTESIAN_POINT ( 'NONE',  ( -23.84209965496292227, -7.976777114481962805, -232.1458837748831456 ) ) ;
#6332 = CARTESIAN_POINT ( 'NONE',  ( -14.24095617957673632, -25.86326826095433162, -229.7068514753157160 ) ) ;
#6333 = CARTESIAN_POINT ( 'NONE',  ( 12.89118769162836031, 6.140251663080722899, -228.8792332048833771 ) ) ;
#6334 = CARTESIAN_POINT ( 'NONE',  ( 0.000000000000000000, 0.000000000000000000, 75.00000000000000000 ) ) ;
#6335 = CARTESIAN_POINT ( 'NONE',  ( -18.17591565587962776, 16.23604867791855355, -233.2845329962925121 ) ) ;
#6336 = CARTESIAN_POINT ( 'NONE',  ( 14.91731358302415877, 13.33846450914490056, -217.2468882285060658 ) ) ;
#6337 = CARTESIAN_POINT ( 'NONE',  ( 4.301648988406530094, 13.23079486486395240, -223.2766268961034655 ) ) ;
#6338 = CARTESIAN_POINT ( 'NONE',  ( 7.017641603801325623, 14.96204511409594673, -228.1064041248110073 ) ) ;
#6339 = CARTESIAN_POINT ( 'NONE',  ( 8.134488596945347538, -11.59059696487595481, -231.6292735970982335 ) ) ;
#6340 = CARTESIAN_POINT ( 'NONE',  ( 27.13894094332088969, 12.30518789341946295, -220.2765066586875093 ) ) ;
#6341 = CARTESIAN_POINT ( 'NONE',  ( -12.80756961294691010, 26.82110654133967387, -223.7464923486294026 ) ) ;
#6342 = CARTESIAN_POINT ( 'NONE',  ( -9.776740361816679936, -16.43846667899986258, -218.0739489017842061 ) ) ;
#6343 = CARTESIAN_POINT ( 'NONE',  ( -20.26851768784797869, -0.8260594303982465858, -217.1279713726092098 ) ) ;
#6344 = DIRECTION ( 'NONE',  ( 0.000000000000000000, 0.000000000000000000, 1.000000000000000000 ) ) ;
#6345 = EDGE_CURVE ( 'NONE', #8548, #1266, #17690, .T. ) ;
#6346 = CARTESIAN_POINT ( 'NONE',  ( 18.50911814746675788, 15.92944434255054453, -232.0449215596906072 ) ) ;
#6347 = CARTESIAN_POINT ( 'NONE',  ( 18.87161431088011199, -9.942086275362749248, -230.8324498438813350 ) ) ;
#6348 = CARTESIAN_POINT ( 'NONE',  ( -12.62195384480319582, 9.244619650382723819, -228.6283004876635516 ) ) ;
#6349 = CARTESIAN_POINT ( 'NONE',  ( -8.376153411442972541, -27.59911039556260448, -219.0729038785590888 ) ) ;
#6350 = CARTESIAN_POINT ( 'NONE',  ( -0.3969026096611234511, 20.89748314411456676, -216.3289738411752978 ) ) ;
#6351 = CARTESIAN_POINT ( 'NONE',  ( 3.044038000507106378, 30.22621415828681180, -231.1553244844465382 ) ) ;
#6352 = ORIENTED_EDGE ( 'NONE', *, *, #10914, .F. ) ;
#6353 = CARTESIAN_POINT ( 'NONE',  ( 2.837900457371055563, 25.11342719071438978, -232.9871906064174709 ) ) ;
#6354 = CARTESIAN_POINT ( 'NONE',  ( 29.78177645116457128, -4.041743286679309044, -225.6339783681140432 ) ) ;
#6355 = CARTESIAN_POINT ( 'NONE',  ( 24.68983475587330645, -0.6584631617853404784, -233.6195837498767958 ) ) ;
#6356 = LINE ( 'NONE', #11534, #6984 ) ;
#6357 = CARTESIAN_POINT ( 'NONE',  ( 4.343013938751969505, 13.02036404005131587, -224.7825435359082178 ) ) ;
#6358 = CARTESIAN_POINT ( 'NONE',  ( -12.24325066776002657, -20.13554689852184509, -214.7483342848939856 ) ) ;
#6359 = CARTESIAN_POINT ( 'NONE',  ( 10.40291689048662782, -13.87512507945592333, -231.9656913702303029 ) ) ;
#6360 = CARTESIAN_POINT ( 'NONE',  ( 14.98777556431132219, -10.10815648641214004, -217.9795565018743844 ) ) ;
#6361 = CARTESIAN_POINT ( 'NONE',  ( -20.04070223234628756, 18.12164545743767263, -231.9292141396248610 ) ) ;
#6362 = CARTESIAN_POINT ( 'NONE',  ( 5.909674498212842408, 15.76475534640655773, -228.4922217450045139 ) ) ;
#6363 = CARTESIAN_POINT ( 'NONE',  ( -28.17543631911187063, 3.557555778861649642, -230.1980773687482156 ) ) ;
#6364 = CARTESIAN_POINT ( 'NONE',  ( -16.65220264499505376, 11.77543314451157563, -216.3149620944649030 ) ) ;
#6365 = CARTESIAN_POINT ( 'NONE',  ( -26.50758677328550306, -10.71756779952945671, -226.4207925882492987 ) ) ;
#6366 = ORIENTED_EDGE ( 'NONE', *, *, #21188, .F. ) ;
#6367 = CARTESIAN_POINT ( 'NONE',  ( -22.07068341299880743, 18.38202870573248049, -227.7785760498121306 ) ) ;
#6368 = CARTESIAN_POINT ( 'NONE',  ( 9.336393807558161839, 27.79372469574263960, -228.5913636680961361 ) ) ;
#6369 = CARTESIAN_POINT ( 'NONE',  ( -6.496078068315311427, 23.46891392553531119, -233.1042179568201220 ) ) ;
#6370 = CARTESIAN_POINT ( 'NONE',  ( 23.33467929415965614, -0.4823873731835089940, -233.9427286327415629 ) ) ;
#6371 = DIRECTION ( 'NONE',  ( 0.000000000000000000, -1.000000000000000000, 0.000000000000000000 ) ) ;
#6372 = ORIENTED_EDGE ( 'NONE', *, *, #10264, .F. ) ;
#6373 = CARTESIAN_POINT ( 'NONE',  ( -9.443239614166923701, 9.388015667058336788, -222.3195230688234290 ) ) ;
#6374 = CARTESIAN_POINT ( 'NONE',  ( -3.917974041549708630, -18.23196399112299559, -217.4080104222929606 ) ) ;
#6375 = CARTESIAN_POINT ( 'NONE',  ( 27.40550551777678123, 5.967061366481472895, -228.7463788799179554 ) ) ;
#6376 = CARTESIAN_POINT ( 'NONE',  ( 12.99034161053428349, 11.71468708507361889, -230.9043293568357740 ) ) ;
#6377 = FACE_OUTER_BOUND ( 'NONE', #21008, .T. ) ;
#6378 = CARTESIAN_POINT ( 'NONE',  ( 14.31589812732703670, -5.349901619299376243, -221.2752230612865105 ) ) ;
#6379 = CARTESIAN_POINT ( 'NONE',  ( -21.66801938871533650, 16.28801167444048659, -218.5240035253498547 ) ) ;
#6380 = CARTESIAN_POINT ( 'NONE',  ( 27.84414217501293010, 2.965433895642837214, -221.8999927093654492 ) ) ;
#6381 = DIRECTION ( 'NONE',  ( -0.000000000000000000, -0.000000000000000000, -1.000000000000000000 ) ) ;
#6382 = EDGE_CURVE ( 'NONE', #3862, #10678, #4024, .T. ) ;
#6383 = CARTESIAN_POINT ( 'NONE',  ( 21.56647080447662290, -0.4294288297056042536, -222.0296485764623640 ) ) ;
#6384 = DIRECTION ( 'NONE',  ( 0.000000000000000000, 0.000000000000000000, -1.000000000000000000 ) ) ;
#6385 = CARTESIAN_POINT ( 'NONE',  ( 26.08609146265030176, -9.082777145696592669, -223.3125241607380360 ) ) ;
#6386 = CARTESIAN_POINT ( 'NONE',  ( -12.44777057840899559, -8.577008958641105352, -229.4809580173677830 ) ) ;
#6387 = ADVANCED_FACE ( 'NONE', ( #5520 ), #12398, .F. ) ;
#6388 = CARTESIAN_POINT ( 'NONE',  ( -20.72013996799678637, -9.983843958838708232, 0.6587422018470180385 ) ) ;
#6389 = DIRECTION ( 'NONE',  ( 0.000000000000000000, 0.000000000000000000, -1.000000000000000000 ) ) ;
#6390 = CARTESIAN_POINT ( 'NONE',  ( 6.332229114051408203, 16.75791367489523154, -229.7702805136205200 ) ) ;
#6391 = ADVANCED_FACE ( 'NONE', ( #19251 ), #12065, .F. ) ;
#6392 = CARTESIAN_POINT ( 'NONE',  ( 13.50228739682142454, -27.74890714798514679, -227.9743917065363519 ) ) ;
#6393 = CARTESIAN_POINT ( 'NONE',  ( 27.32546652195855685, -7.354568365469916991, -229.0866163655393279 ) ) ;
#6394 = CARTESIAN_POINT ( 'NONE',  ( -12.33203608746942237, 8.428128317385924717, -222.9277009507565026 ) ) ;
#6395 = CARTESIAN_POINT ( 'NONE',  ( 29.11492790716816614, 6.132849117128307270, -229.8316941169402412 ) ) ;
#6396 = CARTESIAN_POINT ( 'NONE',  ( 23.44063276014420794, 13.61134749381700182, -229.1061940987080732 ) ) ;
#6397 = ORIENTED_EDGE ( 'NONE', *, *, #3880, .T. ) ;
#6398 = CARTESIAN_POINT ( 'NONE',  ( 4.286954182150454429, -15.41507397180808425, -219.0323159710399352 ) ) ;
#6399 = DIRECTION ( 'NONE',  ( -1.000000000000000000, 0.000000000000000000, 0.000000000000000000 ) ) ;
#6400 = CARTESIAN_POINT ( 'NONE',  ( -18.67456582549428390, 11.07053394491094345, -214.7114755712704550 ) ) ;
#6401 = ORIENTED_EDGE ( 'NONE', *, *, #1237, .F. ) ;
#6402 = CARTESIAN_POINT ( 'NONE',  ( 7.739849882373770917, 11.59357455229016409, -219.5521933286238720 ) ) ;
#6403 = CARTESIAN_POINT ( 'NONE',  ( -2.218529449563984901, 24.06491599887877442, -214.8915873797660652 ) ) ;
#6404 = CARTESIAN_POINT ( 'NONE',  ( 22.90686649137879627, -15.60507238429272192, -227.8443525802422585 ) ) ;
#6405 = CARTESIAN_POINT ( 'NONE',  ( 0.7245137624042983227, 13.44764381486384330, -223.4043886706536455 ) ) ;
#6406 = CARTESIAN_POINT ( 'NONE',  ( -16.20072894238734307, 0.5024448614660336210, -230.4554067149722130 ) ) ;
#6407 = VECTOR ( 'NONE', #9398, 1000.000000000000000 ) ;
#6408 = CARTESIAN_POINT ( 'NONE',  ( 11.13671218404335761, 30.21738803452449673, -224.2405745632392211 ) ) ;
#6409 = CARTESIAN_POINT ( 'NONE',  ( -15.61959985466312872, 8.133362592386543355, -230.7826037412100106 ) ) ;
#6410 = CARTESIAN_POINT ( 'NONE',  ( -2.958555384449997661, 13.07587799061801093, -222.7767538261418565 ) ) ;
#6411 = CARTESIAN_POINT ( 'NONE',  ( 19.72515656911863147, 14.02277373989196541, -218.0718040828188009 ) ) ;
#6412 = CARTESIAN_POINT ( 'NONE',  ( 15.03112630398312177, 24.11065413595933293, -226.8236212149936080 ) ) ;
#6413 = DIRECTION ( 'NONE',  ( 1.000000000000000000, 0.000000000000000000, 0.000000000000000000 ) ) ;
#6414 = DIRECTION ( 'NONE',  ( 1.000000000000000000, 0.000000000000000000, 0.000000000000000000 ) ) ;
#6415 = CARTESIAN_POINT ( 'NONE',  ( -15.51091956967506391, -1.782849713491490018, -228.8089183834494520 ) ) ;
#6416 = CARTESIAN_POINT ( 'NONE',  ( 12.85408565574548412, 7.821283853063205171, -223.1248833997948111 ) ) ;
#6417 = CARTESIAN_POINT ( 'NONE',  ( 0.4137397183702169468, -14.31347623323147289, -219.6167997211809393 ) ) ;
#6418 = CARTESIAN_POINT ( 'NONE',  ( 0.000000000000000000, 0.000000000000000000, -75.00000000000000000 ) ) ;
#6419 = CARTESIAN_POINT ( 'NONE',  ( -8.435479365662203577, 14.12888021429238528, -220.5365774424437859 ) ) ;
#6420 = CARTESIAN_POINT ( 'NONE',  ( 9.009845654114897684, -15.13764346805314354, -231.2790349225496129 ) ) ;
#6421 = CARTESIAN_POINT ( 'NONE',  ( 13.64836464229338198, 15.83060743948028737, -232.0893758582176929 ) ) ;
#6422 = CARTESIAN_POINT ( 'NONE',  ( -10.32994309255856535, 16.55762392127841665, -218.3313395458419279 ) ) ;
#6424 = AXIS2_PLACEMENT_3D ( 'NONE', #5818, #19543, #1087 ) ;
#6423 = CARTESIAN_POINT ( 'NONE',  ( -5.383332542724544645, 15.12651309054520432, -231.5699995578976313 ) ) ;
#6425 = ORIENTED_EDGE ( 'NONE', *, *, #11026, .F. ) ;
#6426 = CARTESIAN_POINT ( 'NONE',  ( -14.92584319327083442, -9.764953932613968490, -229.6443584147421006 ) ) ;
#6427 = CARTESIAN_POINT ( 'NONE',  ( 22.17049319811867036, 0.5483778423327810847, -216.5715983009590673 ) ) ;
#6428 = PRODUCT_DEFINITION ( 'UNKNOWN', '', #10679, #4682 ) ;
#6429 = DIRECTION ( 'NONE',  ( -1.000000000000000000, 0.000000000000000000, -0.000000000000000000 ) ) ;
#6430 = CARTESIAN_POINT ( 'NONE',  ( -17.75199675706278413, -2.086992369311378326, -216.9839424855219931 ) ) ;
#6431 = CARTESIAN_POINT ( 'NONE',  ( 12.95792863868717149, 16.83236386576623644, -216.3406066345214356 ) ) ;
#6432 = CARTESIAN_POINT ( 'NONE',  ( -19.33106196848021341, 9.919700385716687663, -219.0532654734256255 ) ) ;
#6433 = CARTESIAN_POINT ( 'NONE',  ( -2.047892494109819328, 12.88402507277750786, -223.5104301352110951 ) ) ;
#6434 = CARTESIAN_POINT ( 'NONE',  ( 16.20788843645364352, 6.828976201867700269, -231.6689701909764665 ) ) ;
#6435 = CARTESIAN_POINT ( 'NONE',  ( -20.34211109426514597, -24.21145056749966074, -225.0780941718357724 ) ) ;
#6436 = ORIENTED_EDGE ( 'NONE', *, *, #20861, .T. ) ;
#6437 = CARTESIAN_POINT ( 'NONE',  ( -13.66944713747931139, -25.56883467164384527, -222.3908458502962731 ) ) ;
#6438 = CARTESIAN_POINT ( 'NONE',  ( -13.09048442463468120, -0.002406630494250819839, -229.7150300986316438 ) ) ;
#6439 = CARTESIAN_POINT ( 'NONE',  ( 12.02378739738799140, -16.98783239109716092, -233.4545636224233931 ) ) ;
#6440 = CARTESIAN_POINT ( 'NONE',  ( -16.64477864544768337, -2.947896226079009807, -219.6737919733007516 ) ) ;
#6441 = CARTESIAN_POINT ( 'NONE',  ( -22.23616899077527975, -11.51447210886970751, -217.5950109096934568 ) ) ;
#6442 = CARTESIAN_POINT ( 'NONE',  ( 19.13999328532042910, 9.776920959053244431, -216.1190985676915375 ) ) ;
#6443 = DIRECTION ( 'NONE',  ( -0.000000000000000000, -0.000000000000000000, 1.000000000000000000 ) ) ;
#6444 = CARTESIAN_POINT ( 'NONE',  ( -13.71158422780231056, 12.21432067443984693, -232.9166272955793033 ) ) ;
#6445 = CARTESIAN_POINT ( 'NONE',  ( 11.35656094503625901, 14.01405796444069018, -230.6944611846958537 ) ) ;
#6446 = CARTESIAN_POINT ( 'NONE',  ( 4.603870848087811218, 30.13529352683433515, -225.9623629403671430 ) ) ;
#6447 = CARTESIAN_POINT ( 'NONE',  ( 12.14863411169100971, 10.95505907656739097, -219.3725293661985063 ) ) ;
#6448 = CARTESIAN_POINT ( 'NONE',  ( 12.92161125358352791, -8.797851723037126703, -217.2061419145261425 ) ) ;
#6449 = CARTESIAN_POINT ( 'NONE',  ( -10.10782416658048710, 9.083762506436128703, -227.1045422723873344 ) ) ;
#6450 = CARTESIAN_POINT ( 'NONE',  ( -0.7286890422672397394, 21.00519367000705273, -234.2149015821977969 ) ) ;
#6451 = CARTESIAN_POINT ( 'NONE',  ( -12.50828242918857036, -25.45147276965577277, -228.7626325223041022 ) ) ;
#6452 = CARTESIAN_POINT ( 'NONE',  ( -13.92046207272054303, -0.1600067567908077248, -224.5811699126800818 ) ) ;
#6453 = CARTESIAN_POINT ( 'NONE',  ( 0.000000000000000000, 0.000000000000000000, 77.51594804401857175 ) ) ;
#6454 = EDGE_CURVE ( 'NONE', #14043, #20674, #3714, .T. ) ;
#6455 = CARTESIAN_POINT ( 'NONE',  ( 14.85123888640019452, 5.067529763532427012, -221.9058491819374979 ) ) ;
#6456 = CARTESIAN_POINT ( 'NONE',  ( 15.55571562362403704, -22.93410568583619025, -228.9591035895856805 ) ) ;
#6457 = CARTESIAN_POINT ( 'NONE',  ( -13.97943781666340790, 5.798109546139844639, -228.2992319913466019 ) ) ;
#6458 = CARTESIAN_POINT ( 'NONE',  ( 5.359747511823000465, 20.14556701535824601, -232.9094821222151381 ) ) ;
#6459 = CARTESIAN_POINT ( 'NONE',  ( -12.14186164972853810, -9.217338937739926408, -220.4665480714278374 ) ) ;
#6460 = ITEM_DEFINED_TRANSFORMATION ( 'NONE', 'NONE', #14269,  #6677 ) ;
#6461 = CARTESIAN_POINT ( 'NONE',  ( 13.93840998928060415, 0.7705246578886114639, -220.8158265847476116 ) ) ;
#6462 = CARTESIAN_POINT ( 'NONE',  ( 14.28815361401014172, 13.86049093364188778, -216.0585456615740156 ) ) ;
#6463 = ORIENTED_EDGE ( 'NONE', *, *, #22062, .T. ) ;
#6464 = CARTESIAN_POINT ( 'NONE',  ( -5.807479211365208727, 19.77444019604324410, -216.0778658752277863 ) ) ;
#6465 = CARTESIAN_POINT ( 'NONE',  ( 17.73959705210031146, -11.46016327460725748, -231.4839417819510459 ) ) ;
#6466 = CARTESIAN_POINT ( 'NONE',  ( -25.00000000000000355, -0.3291058866677926686, 10.00000000000000178 ) ) ;
#6467 = CARTESIAN_POINT ( 'NONE',  ( 0.000000000000000000, 25.00000000000000000, 75.00000000000000000 ) ) ;
#6468 = CARTESIAN_POINT ( 'NONE',  ( 4.883314309504700468, 19.06839645569368358, -217.0171359871271193 ) ) ;
#6469 = CARTESIAN_POINT ( 'NONE',  ( -14.97068153222459408, -28.62142063984003215, -225.0224449979507142 ) ) ;
#6470 = CARTESIAN_POINT ( 'NONE',  ( 10.10435529162921853, -13.32996982371095918, -231.5224098423250894 ) ) ;
#6471 = DIRECTION ( 'NONE',  ( -0.000000000000000000, 0.000000000000000000, -1.000000000000000000 ) ) ;
#6472 = CARTESIAN_POINT ( 'NONE',  ( -20.80338291456855870, 18.97067006663518995, -230.9007617602332516 ) ) ;
#6473 = CARTESIAN_POINT ( 'NONE',  ( 10.48640380280471618, 25.27581435651469022, -227.8976696013017715 ) ) ;
#6474 = FACE_OUTER_BOUND ( 'NONE', #21415, .T. ) ;
#6475 = CARTESIAN_POINT ( 'NONE',  ( -19.94037810645588138, 20.40093185429846656, -220.0593903119159620 ) ) ;
#6476 = CARTESIAN_POINT ( 'NONE',  ( -18.52912398332900068, -6.554396152115366192, -218.2980051671528088 ) ) ;
#6477 = ORIENTED_EDGE ( 'NONE', *, *, #1436, .F. ) ;
#6478 = CARTESIAN_POINT ( 'NONE',  ( -10.84440549681320221, 27.00404139634608214, -224.0969657459751261 ) ) ;
#6479 = CARTESIAN_POINT ( 'NONE',  ( 22.73582563804385970, 20.20868311426415431, -227.8513184012435886 ) ) ;
#6480 = CARTESIAN_POINT ( 'NONE',  ( 1.984991703947643904, 14.51738422979996912, -218.4500278854917781 ) ) ;
#6481 = CARTESIAN_POINT ( 'NONE',  ( 16.07480884343054939, -7.767425703123992164, -217.5935768756353923 ) ) ;
#6482 = ORIENTED_EDGE ( 'NONE', *, *, #1646, .T. ) ;
#6483 = CARTESIAN_POINT ( 'NONE',  ( -14.00380962569832199, 8.747390586476997854, -231.7950903513155936 ) ) ;
#6484 = CARTESIAN_POINT ( 'NONE',  ( -24.53655852862112496, -9.573911656693818273, -234.4221496410225143 ) ) ;
#6485 = FACE_OUTER_BOUND ( 'NONE', #17914, .T. ) ;
#6486 = CARTESIAN_POINT ( 'NONE',  ( 12.04687593227112430, 27.54339840196571743, -224.6466266724203820 ) ) ;
#6487 = DIRECTION ( 'NONE',  ( -1.000000000000000000, 0.000000000000000000, 0.000000000000000000 ) ) ;
#6488 = LINE ( 'NONE', #4683, #223 ) ;
#6489 = FILL_AREA_STYLE_COLOUR ( '', #2335 ) ;
#6490 = CARTESIAN_POINT ( 'NONE',  ( -14.87984907657228639, 0.2138881189739126887, -228.7773920408832282 ) ) ;
#6491 = CARTESIAN_POINT ( 'NONE',  ( -16.48591407464216729, 7.092323989942422635, -218.8909951703408012 ) ) ;
#6492 = CARTESIAN_POINT ( 'NONE',  ( 13.15438416660314225, 5.520603777723624539, -227.0878346348094681 ) ) ;
#6493 =( NAMED_UNIT ( * ) PLANE_ANGLE_UNIT ( ) SI_UNIT ( $, .RADIAN. ) );
#6494 = CARTESIAN_POINT ( 'NONE',  ( 2.465190328815661892E-29, 25.00000000000012790, 75.00000000000000000 ) ) ;
#6495 = CARTESIAN_POINT ( 'NONE',  ( 14.98418162551161714, 4.450317369940187895, -227.9894155827521161 ) ) ;
#6496 = DIRECTION ( 'NONE',  ( 0.000000000000000000, 0.000000000000000000, 1.000000000000000000 ) ) ;
#6497 = CARTESIAN_POINT ( 'NONE',  ( 23.75342044390781027, -1.773323855525749781, -231.1605140052801630 ) ) ;
#6499 = EDGE_CURVE ( 'NONE', #21649, #17512, #13883, .T. ) ;
#6498 = CARTESIAN_POINT ( 'NONE',  ( -16.39524763169126942, -10.97410814576847926, -232.9630882351523837 ) ) ;
#6500 = CARTESIAN_POINT ( 'NONE',  ( -21.51775537703705155, -8.125520501844063048, -5.837995551681642858 ) ) ;
#6501 = CYLINDRICAL_SURFACE ( 'NONE', #19856, 4.100000000000000533 ) ;
#6502 = CARTESIAN_POINT ( 'NONE',  ( 5.142103055192286831, 28.18228231877369439, -225.8998064704803994 ) ) ;
#6503 = CARTESIAN_POINT ( 'NONE',  ( 19.43707201973751708, -21.22621598813149646, -232.3303264720597667 ) ) ;
#6504 = CARTESIAN_POINT ( 'NONE',  ( 10.99893791904045415, -12.61823049403341201, -218.3266956685045841 ) ) ;
#6505 = VERTEX_POINT ( 'NONE', #21792 ) ;
#6506 = CARTESIAN_POINT ( 'NONE',  ( -12.78923236353123727, 15.53885160143439315, -231.8946633672937878 ) ) ;
#6507 = CARTESIAN_POINT ( 'NONE',  ( 12.23284375931666013, 4.108221165122169616, -224.0993108960438462 ) ) ;
#6508 = CARTESIAN_POINT ( 'NONE',  ( 16.23850682336481199, 8.051046992137072422, -219.2473483181185827 ) ) ;
#6509 = ORIENTED_EDGE ( 'NONE', *, *, #11837, .F. ) ;
#6510 = CARTESIAN_POINT ( 'NONE',  ( -6.954422770286640798, -15.70181985945210634, -221.3390676453758488 ) ) ;
#6511 = CARTESIAN_POINT ( 'NONE',  ( -14.49716617963121834, 0.4310340159982911645, 92.99999999999997158 ) ) ;
#6512 = CARTESIAN_POINT ( 'NONE',  ( -15.39319649241581800, 0.3563955590804028795, -232.4397289486159082 ) ) ;
#6513 = CARTESIAN_POINT ( 'NONE',  ( 9.100443535964535258, 24.01370002727352215, -234.5397711707082635 ) ) ;
#6514 = CARTESIAN_POINT ( 'NONE',  ( 27.02504508796729255, -10.76203424748690907, -225.6681254905965943 ) ) ;
#6515 = EDGE_CURVE ( 'NONE', #9399, #11804, #9576, .T. ) ;
#6516 = CARTESIAN_POINT ( 'NONE',  ( 4.340445191644851874, 29.86837761166362881, -227.4879512554873315 ) ) ;
#6517 = CARTESIAN_POINT ( 'NONE',  ( -17.88126539071149779, 5.766250685202066961, -232.9050303536861293 ) ) ;
#6518 = B_SPLINE_CURVE_WITH_KNOTS ( 'NONE', 3,
 ( #16864, #3338, #22251, #13712, #18985, #15180, #1439, #10109, #12020, #10442, #8429, #8312, #13830, #10220, #13486, #20326, #20440, #87, #8541, #15405, #5138, #18878, #3454, #11799, #4923, #20666, #18666, #3226, #16974, #1553, #10333, #1772, #8646, #12130, #15507, #6958, #3564, #17302, #8761, #15621, #2429, #21110, #9312, #743, #10670, #17422, #17867, #17640 ),
 .UNSPECIFIED., .F., .F.,
 ( 4, 2, 2, 2, 2, 2, 2, 2, 2, 2, 2, 2, 2, 2, 2, 2, 2, 2, 2, 2, 2, 2, 2, 4 ),
 ( 0.004817815020603932220, 0.005107125076144584247, 0.005396435131685235406, 0.005685745187225887433, 0.005975055242766539459, 0.006553675353847844380, 0.006842985409388494672, 0.007132295464929145831, 0.007710915576010501926, 0.008289535687091858021, 0.008868155798173214116, 0.009446775909254571946, 0.01002539602033592978, 0.01060401613141728414, 0.01118263624249864197, 0.01176125635357999979, 0.01205056640912068044, 0.01233987646466135762, 0.01262918652020203827, 0.01291849657574271892, 0.01320780663128339610, 0.01349711668682407675, 0.01378642674236475740, 0.01407573679790543458 ),
 .UNSPECIFIED. ) ;
#6519 = CARTESIAN_POINT ( 'NONE',  ( 8.036750260989780514, 26.29729070384984624, -233.5018314387838529 ) ) ;
#6520 = CARTESIAN_POINT ( 'NONE',  ( -27.01279207917464475, 4.316569700791554887, -221.4451031230926219 ) ) ;
#6521 = CARTESIAN_POINT ( 'NONE',  ( -3.501680520304516264, 14.31538576447642264, -219.8967178229432307 ) ) ;
#6522 = CARTESIAN_POINT ( 'NONE',  ( -7.157650466794449606, 8.055668064929562888, 92.00000000000001421 ) ) ;
#6523 = CARTESIAN_POINT ( 'NONE',  ( 14.96080648943632241, 22.28365808184747721, -220.1237743409445216 ) ) ;
#6524 = CARTESIAN_POINT ( 'NONE',  ( 17.50000000000000355, 0.000000000000000000, -25.00000000000000000 ) ) ;
#6525 = DIRECTION ( 'NONE',  ( -1.000000000000000000, 0.000000000000000000, 0.000000000000000000 ) ) ;
#6526 = LINE ( 'NONE', #10027, #13387 ) ;
#6527 = CARTESIAN_POINT ( 'NONE',  ( 27.04607490430786854, 4.607450003618843049, -220.3758934308003461 ) ) ;
#6528 = CARTESIAN_POINT ( 'NONE',  ( -13.13160344394316503, -9.470348871083606568, -223.0142826039989075 ) ) ;
#6529 = CARTESIAN_POINT ( 'NONE',  ( 2.999999999999972466, -6.000000000000006217, -221.9999999999999716 ) ) ;
#6530 = CIRCLE ( 'NONE', #9416, 2.000000000000000000 ) ;
#6531 = CARTESIAN_POINT ( 'NONE',  ( -9.661739055621840322, 20.41227307912577871, -232.0920144483423257 ) ) ;
#6532 =( NAMED_UNIT ( * ) SI_UNIT ( $, .STERADIAN. ) SOLID_ANGLE_UNIT ( ) );
#6533 = CARTESIAN_POINT ( 'NONE',  ( 3.619268272960482591, -21.10655420957111517, -217.8630709410095108 ) ) ;
#6534 = CARTESIAN_POINT ( 'NONE',  ( 14.91731358302415877, 13.33846450914490056, -217.2468882285060658 ) ) ;
#6535 = CARTESIAN_POINT ( 'NONE',  ( -4.466732464217805898, 19.42663028452474450, -231.9485309169485561 ) ) ;
#6536 = CARTESIAN_POINT ( 'NONE',  ( -5.298027976154672025, 13.43376398981453157, -220.6333279128949982 ) ) ;
#6537 = CARTESIAN_POINT ( 'NONE',  ( -24.13163560393529394, -13.84165259829251227, -223.2936513752361805 ) ) ;
#6538 = EDGE_CURVE ( 'NONE', #1838, #17384, #6488, .T. ) ;
#6539 = CARTESIAN_POINT ( 'NONE',  ( 8.812073984913094904, 13.12649198322903210, -229.9172071780580495 ) ) ;
#6540 = CARTESIAN_POINT ( 'NONE',  ( -28.00010259152825398, 3.831607968041374157, -225.8381323513402208 ) ) ;
#6541 = CIRCLE ( 'NONE', #18035, 3.000000000000002665 ) ;
#6542 = CARTESIAN_POINT ( 'NONE',  ( 0.000000000000000000, 0.000000000000000000, -74.48236190979496030 ) ) ;
#6543 = CARTESIAN_POINT ( 'NONE',  ( -14.73876579896802141, -0.4225899574144328374, -230.2531052195884342 ) ) ;
#6544 = CARTESIAN_POINT ( 'NONE',  ( 13.20340559785743828, 9.575208899273587093, -218.1210831379648312 ) ) ;
#6545 = CARTESIAN_POINT ( 'NONE',  ( -22.90687623753526125, 9.466200233939549236, -230.1557007022273638 ) ) ;
#6546 = CARTESIAN_POINT ( 'NONE',  ( 8.546572992885776543, 19.06776382077057974, -214.7173484156796519 ) ) ;
#6547 = CARTESIAN_POINT ( 'NONE',  ( 23.83082175545800752, 15.77842900014857896, -219.5351905769044834 ) ) ;
#6548 = ORIENTED_EDGE ( 'NONE', *, *, #7297, .F. ) ;
#6549 = CARTESIAN_POINT ( 'NONE',  ( -8.875208054371373834, -23.27682998066124398, -233.1222812539844540 ) ) ;
#6550 = TOROIDAL_SURFACE ( 'NONE', #2248, 24.63401512838748530, 3.000000000000004441 ) ;
#6551 = ORIENTED_EDGE ( 'NONE', *, *, #18200, .T. ) ;
#6552 = CARTESIAN_POINT ( 'NONE',  ( -10.03082531488024109, -22.09229706162428286, -231.9736132431984572 ) ) ;
#6553 = CARTESIAN_POINT ( 'NONE',  ( -21.85741505224184777, 1.741064654082184582, -235.1654459941842390 ) ) ;
#6554 = CARTESIAN_POINT ( 'NONE',  ( 13.47054497134856277, -24.75371201277411615, -218.7687119198782000 ) ) ;
#6555 = CARTESIAN_POINT ( 'NONE',  ( 11.88751558872989378, -3.770303194171726435, -225.3699946362665969 ) ) ;
#6556 = CARTESIAN_POINT ( 'NONE',  ( -20.85586116824185510, -1.996934699305910499, -232.3804859832740135 ) ) ;
#6557 = CARTESIAN_POINT ( 'NONE',  ( 25.40172858355122898, 15.07073195964820833, -229.0276483847865450 ) ) ;
#6558 = DIRECTION ( 'NONE',  ( -0.000000000000000000, 0.000000000000000000, -1.000000000000000000 ) ) ;
#6559 = CARTESIAN_POINT ( 'NONE',  ( -15.57505478537380306, 24.84242291948262249, -225.5907943047649837 ) ) ;
#6560 = CARTESIAN_POINT ( 'NONE',  ( 12.49127101283658803, 6.474961340449192804, -221.2149164507559078 ) ) ;
#6561 = CARTESIAN_POINT ( 'NONE',  ( 15.33737796850231305, 13.57479350230705428, -232.3313557812109025 ) ) ;
#6562 = CARTESIAN_POINT ( 'NONE',  ( 8.778334628954494789, 12.71782457734010841, -222.1923057070808909 ) ) ;
#6563 = CARTESIAN_POINT ( 'NONE',  ( 22.36312131198404174, -23.32398317548372546, -224.0789201928890861 ) ) ;
#6564 = CARTESIAN_POINT ( 'NONE',  ( -2.917590128672695293, 18.81591489065672818, -216.3635620530855022 ) ) ;
#6565 = ADVANCED_FACE ( 'NONE', ( #2995 ), #14510, .F. ) ;
#6566 = DIRECTION ( 'NONE',  ( -0.000000000000000000, -0.000000000000000000, 1.000000000000000000 ) ) ;
#6567 = AXIS2_PLACEMENT_3D ( 'NONE', #9269, #17707, #809 ) ;
#6568 = CARTESIAN_POINT ( 'NONE',  ( -17.50000000000007816, 0.000000000000000000, -24.99999999999999645 ) ) ;
#6569 = VECTOR ( 'NONE', #14962, 1000.000000000000000 ) ;
#6570 = CARTESIAN_POINT ( 'NONE',  ( 10.83706092800007781, 10.12544885278926543, -227.1716144446442343 ) ) ;
#6571 = CARTESIAN_POINT ( 'NONE',  ( 3.737871636182809265, -14.23896033977216113, -229.0757302894822942 ) ) ;
#6572 = CARTESIAN_POINT ( 'NONE',  ( -26.38808873681881906, 13.30696350521622939, -225.1492950792419663 ) ) ;
#6573 = CARTESIAN_POINT ( 'NONE',  ( 3.160467108836292116, 14.95099014189016629, -228.9242958482614370 ) ) ;
#6574 = CARTESIAN_POINT ( 'NONE',  ( -13.67406442719345883, -9.319000780081536206, -231.1492214949047934 ) ) ;
#6575 = ITEM_DEFINED_TRANSFORMATION ( 'NONE', 'NONE', #13909,  #6677 ) ;
#6576 = CARTESIAN_POINT ( 'NONE',  ( -23.52458685063474420, 4.195399146287285497, -230.7490123595086970 ) ) ;
#6577 = CARTESIAN_POINT ( 'NONE',  ( 20.05374812456133782, 24.17492691056345677, -223.1494843338164458 ) ) ;
#6578 = EDGE_LOOP ( 'NONE', ( #14497, #16847 ) ) ;
#6579 = CARTESIAN_POINT ( 'NONE',  ( -0.1571923090946999446, 19.34188126963334398, -216.6893131123363787 ) ) ;
#6580 = CARTESIAN_POINT ( 'NONE',  ( 13.61677703237491777, -11.64725695657166682, -220.6715806775949034 ) ) ;
#6581 = CARTESIAN_POINT ( 'NONE',  ( 24.14841045621385263, -15.62485098017456586, -229.9279278555176518 ) ) ;
#6582 = DIRECTION ( 'NONE',  ( -0.000000000000000000, -0.000000000000000000, 1.000000000000000000 ) ) ;
#6583 = CARTESIAN_POINT ( 'NONE',  ( 6.093530912645064745, 16.79941505724243811, -232.1766444656230419 ) ) ;
#6584 = CARTESIAN_POINT ( 'NONE',  ( -12.06899374386015644, -4.263779665926158202, -221.6855044605631520 ) ) ;
#6585 = CARTESIAN_POINT ( 'NONE',  ( 5.609436632608550966, -13.11664087352601094, -229.3324225951633650 ) ) ;
#6586 = AXIS2_PLACEMENT_3D ( 'NONE', #12281, #19766, #5937 ) ;
#6587 = CARTESIAN_POINT ( 'NONE',  ( 14.99336262864975211, -23.54026314425397004, -231.3018640253376361 ) ) ;
#6588 = VECTOR ( 'NONE', #5691, 1000.000000000000000 ) ;
#6589 = CARTESIAN_POINT ( 'NONE',  ( -25.00745438246740804, 14.90779342625281778, -219.2410538611701156 ) ) ;
#6590 = CARTESIAN_POINT ( 'NONE',  ( 14.78510113471881304, 14.77128235908076803, -230.8056908117964383 ) ) ;
#6591 = CARTESIAN_POINT ( 'NONE',  ( -17.88126539071149779, 5.766250685202066961, -232.9050303536861293 ) ) ;
#6592 = CARTESIAN_POINT ( 'NONE',  ( -14.83806045519817829, 13.18806197935771074, -233.4179411789645542 ) ) ;
#6593 = CARTESIAN_POINT ( 'NONE',  ( -14.04666385475200485, -11.54975518965215286, -229.4392169170632201 ) ) ;
#6594 = ORIENTED_EDGE ( 'NONE', *, *, #8422, .T. ) ;
#6595 = CARTESIAN_POINT ( 'NONE',  ( -8.857704405076667342, 24.20848540845601704, -218.8859504303524091 ) ) ;
#6596 = EDGE_CURVE ( 'NONE', #8679, #18055, #6735, .T. ) ;
#6597 = CARTESIAN_POINT ( 'NONE',  ( 11.63337745479824292, 8.229076005436313679, -220.5472098800687206 ) ) ;
#6598 = CARTESIAN_POINT ( 'NONE',  ( 2.165130313308041288, 31.55305250914585002, -225.6791154433767304 ) ) ;
#6599 = CARTESIAN_POINT ( 'NONE',  ( 25.09678678204237201, -16.96620885351193309, -225.7902784465786965 ) ) ;
#6600 = CARTESIAN_POINT ( 'NONE',  ( 22.00000000000000000, 0.000000000000000000, -221.9999999999999716 ) ) ;
#6601 = ORIENTED_EDGE ( 'NONE', *, *, #2906, .F. ) ;
#6602 = CARTESIAN_POINT ( 'NONE',  ( -14.73016414256368911, 22.23431809695627237, -217.1425123644553707 ) ) ;
#6603 = CARTESIAN_POINT ( 'NONE',  ( -8.622882141441040815, -8.945706011589379614, -222.9266619361505377 ) ) ;
#6604 = CYLINDRICAL_SURFACE ( 'NONE', #19110, 17.50000000000000355 ) ;
#6605 = CARTESIAN_POINT ( 'NONE',  ( 18.50911814746675788, 15.92944434255054453, -232.0449215596906072 ) ) ;
#6606 = DIRECTION ( 'NONE',  ( 0.000000000000000000, 0.000000000000000000, -1.000000000000000000 ) ) ;
#6607 = AXIS2_PLACEMENT_3D ( 'NONE', #4143, #11022, #18106 ) ;
#6608 = CARTESIAN_POINT ( 'NONE',  ( 13.28406271702445274, -5.237238614233280742, -225.2640488721434622 ) ) ;
#6609 = CARTESIAN_POINT ( 'NONE',  ( -28.59157645096996347, 5.137867505054540374, -220.4667042235044505 ) ) ;
#6610 = CARTESIAN_POINT ( 'NONE',  ( -12.99458409358603284, 11.56864380452031504, -232.0274663316965018 ) ) ;
#6611 = CARTESIAN_POINT ( 'NONE',  ( 16.31458447723494132, 2.619382102851042671, -229.5862799001085364 ) ) ;
#6612 = CARTESIAN_POINT ( 'NONE',  ( -7.972347216402701164, -18.74702622849856937, -232.1058264431568148 ) ) ;
#6613 = CARTESIAN_POINT ( 'NONE',  ( -2.000000000000000000, 2.449293598294706414E-16, -120.0000000000000142 ) ) ;
#6614 = CARTESIAN_POINT ( 'NONE',  ( 19.02965008953347237, -2.769875716686367007, -223.8421603075141491 ) ) ;
#6615 = CYLINDRICAL_SURFACE ( 'NONE', #3735, 21.00000000000008171 ) ;
#6616 = CARTESIAN_POINT ( 'NONE',  ( 19.27468327664662695, -19.23223527390535637, -221.0469535581208618 ) ) ;
#6617 = CARTESIAN_POINT ( 'NONE',  ( 25.50000000000000000, -0.5000000000000000000, -6.000000000000000000 ) ) ;
#6618 = CARTESIAN_POINT ( 'NONE',  ( -22.97163508793729036, -1.317345109681407722, 9.935299231138023046 ) ) ;
#6619 = CARTESIAN_POINT ( 'NONE',  ( -2.775557561562891351E-14, 0.000000000000000000, -105.0000000000000142 ) ) ;
#6620 = CARTESIAN_POINT ( 'NONE',  ( 10.63406535173453271, 22.16595115341124256, -219.6461356279925781 ) ) ;
#6621 = CARTESIAN_POINT ( 'NONE',  ( 17.90345650676399814, -22.75668921074696982, -218.1849408917474022 ) ) ;
#6622 = CARTESIAN_POINT ( 'NONE',  ( 12.70477135646371281, -9.814387909761604689, -230.3443492180780652 ) ) ;
#6623 = EDGE_LOOP ( 'NONE', ( #14938, #18806 ) ) ;
#6624 = CARTESIAN_POINT ( 'NONE',  ( -17.78731991475362406, 16.78509880370027929, -218.2387321183659310 ) ) ;
#6625 = CARTESIAN_POINT ( 'NONE',  ( -17.29038495093124084, 2.707785585324113065, -229.0475017805649998 ) ) ;
#6626 = CARTESIAN_POINT ( 'NONE',  ( 14.37653162493774239, 9.985418694807894013, -229.1686718965858063 ) ) ;
#6627 = ORIENTED_EDGE ( 'NONE', *, *, #8856, .F. ) ;
#6628 = AXIS2_PLACEMENT_3D ( 'NONE', #18664, #22142, #22249 ) ;
#6629 = CARTESIAN_POINT ( 'NONE',  ( -8.783466540727490113, -25.47690852953548557, -220.9562114332719318 ) ) ;
#6630 = CARTESIAN_POINT ( 'NONE',  ( 0.000000000000000000, 0.000000000000000000, 77.51594804401857175 ) ) ;
#6631 = CARTESIAN_POINT ( 'NONE',  ( -28.12586305337175219, 12.75764838638491305, -230.3810511299127768 ) ) ;
#6632 = CARTESIAN_POINT ( 'NONE',  ( 13.06625079052675531, 10.14096931681969238, -232.1435240729728093 ) ) ;
#6633 = CARTESIAN_POINT ( 'NONE',  ( 9.790069677392189362, -14.58761328102826837, -228.7245293813585647 ) ) ;
#6634 = CARTESIAN_POINT ( 'NONE',  ( 11.82943521288609823, 27.58963564415041247, -226.1180395413371400 ) ) ;
#6635 = CARTESIAN_POINT ( 'NONE',  ( -29.88125065636863198, 4.504452993877526623, -226.2048141718237275 ) ) ;
#6636 = EDGE_CURVE ( 'NONE', #580, #19076, #22144, .T. ) ;
#6637 = CARTESIAN_POINT ( 'NONE',  ( 10.66732316618037402, 25.78610527446713263, -216.5597036843431624 ) ) ;
#6638 = CARTESIAN_POINT ( 'NONE',  ( -13.66744685701839046, 5.938820276054873837, -223.0954633396572149 ) ) ;
#6639 = CARTESIAN_POINT ( 'NONE',  ( -6.101488798441174310, 11.33371047077072369, -225.3616985956418546 ) ) ;
#6640 = CIRCLE ( 'NONE', #13097, 3.000000000000002665 ) ;
#6641 = CARTESIAN_POINT ( 'NONE',  ( 18.06016678184731461, 2.257982981100609354, -218.9983079406065940 ) ) ;
#6642 = CARTESIAN_POINT ( 'NONE',  ( 3.689800395305025127, 23.07294874520714956, -219.2515233573129478 ) ) ;
#6643 = CARTESIAN_POINT ( 'NONE',  ( 28.33476664927451338, -0.7768526459456059907, -228.3750448408243869 ) ) ;
#6644 = FACE_OUTER_BOUND ( 'NONE', #536, .T. ) ;
#6645 = CARTESIAN_POINT ( 'NONE',  ( -22.20848920810297855, -2.028924892417935055, -232.4401719831211039 ) ) ;
#6646 = CARTESIAN_POINT ( 'NONE',  ( 17.07668571305246985, 2.037405138410691485, -219.7626854147787867 ) ) ;
#6647 = CARTESIAN_POINT ( 'NONE',  ( -12.96306772261163154, -8.963621967909368493, -225.1938837381851215 ) ) ;
#6648 = CARTESIAN_POINT ( 'NONE',  ( -3.400000000000003908, 0.000000000000000000, -227.9999999999999716 ) ) ;
#6649 = CARTESIAN_POINT ( 'NONE',  ( -8.030397104878142400, 15.90963402996711373, -230.6518438502475590 ) ) ;
#6650 = PRESENTATION_STYLE_ASSIGNMENT (( #18694 ) ) ;
#6651 = CARTESIAN_POINT ( 'NONE',  ( 1.632321987819951969, -14.78074153629778387, -224.5834756332612301 ) ) ;
#6652 = CARTESIAN_POINT ( 'NONE',  ( 26.51393280883522863, 15.12455065102723495, -226.1955201378414415 ) ) ;
#6653 = CARTESIAN_POINT ( 'NONE',  ( -10.84440549681320221, 27.00404139634608214, -224.0969657459751261 ) ) ;
#6654 = CARTESIAN_POINT ( 'NONE',  ( -16.96626096607909417, 26.06638125783293347, -227.3272535207661349 ) ) ;
#6655 = VERTEX_POINT ( 'NONE', #6617 ) ;
#6656 = CARTESIAN_POINT ( 'NONE',  ( 29.48160760559006732, -8.328447718542550504, -230.7159994440206390 ) ) ;
#6657 = ORIENTED_EDGE ( 'NONE', *, *, #3842, .T. ) ;
#6658 = CARTESIAN_POINT ( 'NONE',  ( 14.31308345469695453, 12.76656023072872159, -231.9445021321040770 ) ) ;
#6659 = CARTESIAN_POINT ( 'NONE',  ( -26.88784739727922357, 10.07520213145270915, -227.1866063047054922 ) ) ;
#6660 = CARTESIAN_POINT ( 'NONE',  ( -16.29666348338687953, 2.994680995215331709, -221.2421885839926006 ) ) ;
#6661 = AXIS2_PLACEMENT_3D ( 'NONE', #17893, #2456, #9666 ) ;
#6662 = DIRECTION ( 'NONE',  ( 1.000000000000000000, -0.000000000000000000, -0.000000000000000000 ) ) ;
#6663 = CARTESIAN_POINT ( 'NONE',  ( -13.18205254385204661, -0.5588607053421433823, -223.2849229087554761 ) ) ;
#6664 = CARTESIAN_POINT ( 'NONE',  ( 8.554868430186942874, 10.42313681336814568, -223.0114508542762621 ) ) ;
#6665 = CARTESIAN_POINT ( 'NONE',  ( -26.35007260221545877, 6.140745174321167177, -221.9336216792591188 ) ) ;
#6666 = CARTESIAN_POINT ( 'NONE',  ( 7.651502705057454889, 16.60422307457919544, -215.4679461133464144 ) ) ;
#6667 = CARTESIAN_POINT ( 'NONE',  ( 18.39533937270110187, 14.26564464607222504, -233.9088367426310242 ) ) ;
#6668 = CARTESIAN_POINT ( 'NONE',  ( -8.622882141441040815, -8.945706011589379614, -222.9266619361505377 ) ) ;
#6669 = ORIENTED_EDGE ( 'NONE', *, *, #13487, .T. ) ;
#6670 = CARTESIAN_POINT ( 'NONE',  ( -5.139154528335864391, -14.05392405596956529, -226.2842807754188641 ) ) ;
#6671 = EDGE_CURVE ( 'NONE', #14415, #12719, #7072, .T. ) ;
#6672 = CARTESIAN_POINT ( 'NONE',  ( -16.95112677453439431, 10.32962960657076934, -214.9445123409346650 ) ) ;
#6673 = CARTESIAN_POINT ( 'NONE',  ( 5.609436632608550966, -13.11664087352601094, -229.3324225951633650 ) ) ;
#6674 = CARTESIAN_POINT ( 'NONE',  ( -3.003186468682855104, 15.63968344752823469, -231.5301608670590667 ) ) ;
#6675 = CARTESIAN_POINT ( 'NONE',  ( 29.76850351104168979, -8.061840962539296385, -221.9850081079297581 ) ) ;
#6676 = CARTESIAN_POINT ( 'NONE',  ( -19.88402822078561627, -6.951120502836210413, -232.7962440186676361 ) ) ;
#6677 = AXIS2_PLACEMENT_3D ( 'NONE', #18028, #16226, #2707 ) ;
#6678 = CARTESIAN_POINT ( 'NONE',  ( 12.49127101283658803, 6.474961340449192804, -221.2149164507559078 ) ) ;
#6679 = DIRECTION ( 'NONE',  ( 1.000000000000000000, 0.000000000000000000, 0.000000000000000000 ) ) ;
#6680 = CARTESIAN_POINT ( 'NONE',  ( -12.67136363292824086, 22.56975222910433843, -219.0840033572168011 ) ) ;
#6681 = CARTESIAN_POINT ( 'NONE',  ( 25.40172858355122898, 15.07073195964820833, -229.0276483847865450 ) ) ;
#6682 = CARTESIAN_POINT ( 'NONE',  ( 11.57669841200422134, 10.63052136557218574, -228.9489978335593889 ) ) ;
#6683 = CARTESIAN_POINT ( 'NONE',  ( 7.249842700832647147, 18.24319783868832801, -219.1110502051974720 ) ) ;
#6684 = CARTESIAN_POINT ( 'NONE',  ( 3.531840179394873491, -11.29480931768500618, -224.5922842895475355 ) ) ;
#6685 = CARTESIAN_POINT ( 'NONE',  ( -5.854583994961135573, 13.10358817970001866, -222.4168379437668648 ) ) ;
#6686 = CARTESIAN_POINT ( 'NONE',  ( -13.69675006931110417, 3.702342960760605539, -228.0723273272095355 ) ) ;
#6687 = CARTESIAN_POINT ( 'NONE',  ( 0.000000000000000000, 22.63401512838754570, 77.51594804401857175 ) ) ;
#6688 = CARTESIAN_POINT ( 'NONE',  ( 8.072455080350884771, -13.51419333260225741, -221.0758372092125228 ) ) ;
#6689 = CARTESIAN_POINT ( 'NONE',  ( -16.81936022032888545, 5.700806722825413786, -218.5726178058217215 ) ) ;
#6690 = AXIS2_PLACEMENT_3D ( 'NONE', #9135, #1210, #574 ) ;
#6691 = CARTESIAN_POINT ( 'NONE',  ( -4.784012432433236484, 23.31984772163034947, -232.0554186943449508 ) ) ;
#6692 = COLOUR_RGB ( '', 0.66274510, 0.83137255, 0.94901961) ;
#6693 = CARTESIAN_POINT ( 'NONE',  ( -14.40111287326894640, -6.123720356435734757, -220.5571602876142094 ) ) ;
#6694 = CARTESIAN_POINT ( 'NONE',  ( 29.11492790716816614, 6.132849117128307270, -229.8316941169402412 ) ) ;
#6695 = CARTESIAN_POINT ( 'NONE',  ( 19.29971334243027314, 24.42889259816135095, -228.2141526116784291 ) ) ;
#6696 = ORIENTED_EDGE ( 'NONE', *, *, #2239, .T. ) ;
#6697 = CARTESIAN_POINT ( 'NONE',  ( -10.45786516112131892, 23.61456281964591852, -233.2869923610001592 ) ) ;
#6698 = CARTESIAN_POINT ( 'NONE',  ( 18.69377297094946755, -6.763382089143314957, -232.1160126380615338 ) ) ;
#6699 = CARTESIAN_POINT ( 'NONE',  ( 15.56514059923893178, -9.210181625211102840, -232.5361143517874325 ) ) ;
#6700 = CARTESIAN_POINT ( 'NONE',  ( -11.33137429837660193, 27.25022425932026238, -230.1650924901870212 ) ) ;
#6701 = LINE ( 'NONE', #1406, #15264 ) ;
#6702 = CARTESIAN_POINT ( 'NONE',  ( 10.66614775643814994, 26.29080367171353672, -230.0818785118670178 ) ) ;
#6703 = CARTESIAN_POINT ( 'NONE',  ( -18.15502857810558268, -5.877683472035677426, -234.3930847616834683 ) ) ;
#6704 = CARTESIAN_POINT ( 'NONE',  ( -11.40116373163465369, -15.95513543764466213, -216.7841692646331353 ) ) ;
#6705 = CARTESIAN_POINT ( 'NONE',  ( 7.958080982411646076, -16.12895853103474408, -217.0903302464454612 ) ) ;
#6706 = CARTESIAN_POINT ( 'NONE',  ( -9.403561938624596550, 12.70246821120386471, -220.7484614495429582 ) ) ;
#6707 = CARTESIAN_POINT ( 'NONE',  ( 16.29563576379945999, 21.41235115595959826, -221.8114656550040991 ) ) ;
#6708 = CARTESIAN_POINT ( 'NONE',  ( -22.04257564474043818, 18.72061943465525857, -219.1781831295219263 ) ) ;
#6709 = CARTESIAN_POINT ( 'NONE',  ( -27.17783334270200157, 15.20409188923851751, -223.6555185980277258 ) ) ;
#6710 = CARTESIAN_POINT ( 'NONE',  ( -14.97948828349161232, -4.621108923465524931, -227.6270126398174796 ) ) ;
#6711 = AXIS2_PLACEMENT_3D ( 'NONE', #5860, #691, #14761 ) ;
#6712 = ORIENTED_EDGE ( 'NONE', *, *, #14581, .F. ) ;
#6713 = CARTESIAN_POINT ( 'NONE',  ( -4.866400999161825780, 25.69921167300892861, -231.0100031340613782 ) ) ;
#6714 = CARTESIAN_POINT ( 'NONE',  ( 10.70175380652492336, 7.370128018021000038, -224.3479584370086286 ) ) ;
#6715 = CARTESIAN_POINT ( 'NONE',  ( 8.865150807857233417, 8.939496441981303221, -220.7647208555746090 ) ) ;
#6716 = CARTESIAN_POINT ( 'NONE',  ( 10.52067862919218832, -10.34113464825721351, -228.4460540958991714 ) ) ;
#6717 = DIRECTION ( 'NONE',  ( 1.000000000000000000, 0.000000000000000000, 0.000000000000000000 ) ) ;
#6718 = ORIENTED_EDGE ( 'NONE', *, *, #20553, .F. ) ;
#6719 = CARTESIAN_POINT ( 'NONE',  ( -3.205260335674071648, 17.52234722004434531, -232.9754319808710363 ) ) ;
#6720 = CARTESIAN_POINT ( 'NONE',  ( -19.24125987773642166, -8.201885216777814236, -235.2928755229699789 ) ) ;
#6721 = EDGE_CURVE ( 'NONE', #6170, #13407, #6518, .T. ) ;
#6722 = DIRECTION ( 'NONE',  ( -1.000000000000000000, 0.000000000000000000, 0.000000000000000000 ) ) ;
#6723 = CARTESIAN_POINT ( 'NONE',  ( 14.22574309452842733, 4.476723532073429546, -225.5862451792618231 ) ) ;
#6724 = CARTESIAN_POINT ( 'NONE',  ( 0.000000000000000000, 0.000000000000000000, 77.51594804401857175 ) ) ;
#6725 = CARTESIAN_POINT ( 'NONE',  ( 11.39114332821395692, -8.257479203742953189, -226.5648397932267528 ) ) ;
#6726 =( NAMED_UNIT ( * ) SI_UNIT ( $, .STERADIAN. ) SOLID_ANGLE_UNIT ( ) );
#6727 = CARTESIAN_POINT ( 'NONE',  ( -24.48580119005125866, 9.312492396273500006, -232.5498413856076070 ) ) ;
#6728 = PRODUCT_DEFINITION_SHAPE ( 'NONE', 'NONE',  #22267 ) ;
#6729 = CARTESIAN_POINT ( 'NONE',  ( 18.69835413980967687, -1.262199651413310031, -230.6153330080101966 ) ) ;
#6730 = CARTESIAN_POINT ( 'NONE',  ( -13.55429797312971374, -24.97278848321653300, -221.1627755146857908 ) ) ;
#6731 = DIRECTION ( 'NONE',  ( 0.000000000000000000, 0.000000000000000000, -1.000000000000000000 ) ) ;
#6732 = CARTESIAN_POINT ( 'NONE',  ( 18.93769218002321253, -2.849225658158391461, -224.0541049803088356 ) ) ;
#6733 = DIRECTION ( 'NONE',  ( -0.000000000000000000, -0.000000000000000000, 1.000000000000000000 ) ) ;
#6734 = CARTESIAN_POINT ( 'NONE',  ( 20.29112488791128399, -13.23242053965672049, -219.3899762660180102 ) ) ;
#6735 = LINE ( 'NONE', #18770, #11723 ) ;
#6736 = CARTESIAN_POINT ( 'NONE',  ( -21.73931781725157464, -7.525425332153104385, 6.616964900418876638 ) ) ;
#6737 = CARTESIAN_POINT ( 'NONE',  ( 9.322595869360968734, 23.38184458253662967, -230.2763482547081821 ) ) ;
#6738 = CARTESIAN_POINT ( 'NONE',  ( 2.482746429915354547, 16.41797261123590346, -229.5599230346982154 ) ) ;
#6739 = CARTESIAN_POINT ( 'NONE',  ( 6.889583945421565048, -13.03635046449108081, -231.0237689561592731 ) ) ;
#6740 = CARTESIAN_POINT ( 'NONE',  ( 13.99926435381047618, -21.11851526759364006, -232.9234173943665951 ) ) ;
#6741 = VERTEX_POINT ( 'NONE', #16173 ) ;
#6742 = CARTESIAN_POINT ( 'NONE',  ( -7.240690404266621805, 13.01623002570985044, -225.3000933658701967 ) ) ;
#6743 = CARTESIAN_POINT ( 'NONE',  ( -21.18474081038989354, 8.486062504918864491, -230.7949373529753530 ) ) ;
#6744 = CARTESIAN_POINT ( 'NONE',  ( 23.24653631066306048, 11.83805845626388020, -219.6020901153134162 ) ) ;
#6745 = VERTEX_POINT ( 'NONE', #5695 ) ;
#6746 = CARTESIAN_POINT ( 'NONE',  ( -8.081326109241135924, -15.70152450856234871, -229.3783721713404304 ) ) ;
#6747 = CARTESIAN_POINT ( 'NONE',  ( 6.688043756404092655, -8.469031667849375111, 92.00000000000000000 ) ) ;
#6748 = ORIENTED_EDGE ( 'NONE', *, *, #756, .T. ) ;
#6749 = CARTESIAN_POINT ( 'NONE',  ( 3.672031556878595282, 11.54613252248376831, -227.4694100414545801 ) ) ;
#6750 = CARTESIAN_POINT ( 'NONE',  ( 17.97642781552999836, -18.85565020944788373, -229.3765379620127760 ) ) ;
#6751 = CARTESIAN_POINT ( 'NONE',  ( 12.53674998645855787, 17.96979015029927851, -232.8843215672231679 ) ) ;
#6752 = CARTESIAN_POINT ( 'NONE',  ( -14.87984907657228639, 0.2138881189739126887, -228.7773920408832282 ) ) ;
#6753 = CARTESIAN_POINT ( 'NONE',  ( 5.784594921161807513, 11.98867617302893329, -219.3746160931291058 ) ) ;
#6754 = CARTESIAN_POINT ( 'NONE',  ( -14.30096418567650041, 6.974026439069829664, -228.7941652905285537 ) ) ;
#6755 = CARTESIAN_POINT ( 'NONE',  ( -7.429838964355703901, 14.87322129099639234, -232.2632863647814077 ) ) ;
#6756 = CARTESIAN_POINT ( 'NONE',  ( 10.76794919243112325, 0.000000000000000000, 92.00000000000000000 ) ) ;
#6757 = CARTESIAN_POINT ( 'NONE',  ( 4.682724365302521896, -22.35092628325669750, -215.9543778044225348 ) ) ;
#6758 = DIRECTION ( 'NONE',  ( -1.000000000000000000, 0.000000000000000000, -0.000000000000000000 ) ) ;
#6759 = DIRECTION ( 'NONE',  ( 0.000000000000000000, 0.000000000000000000, 1.000000000000000000 ) ) ;
#6760 = CARTESIAN_POINT ( 'NONE',  ( -27.09167109716269550, -0.2825935922571593539, -219.8389404328913486 ) ) ;
#6761 = CARTESIAN_POINT ( 'NONE',  ( 17.34727976380017722, 4.822939981779328811, -230.8836217450937909 ) ) ;
#6762 = CARTESIAN_POINT ( 'NONE',  ( -12.44262610342426711, -20.67338498558408588, -232.3867413080560027 ) ) ;
#6763 = CARTESIAN_POINT ( 'NONE',  ( 21.82670294635401831, 0.1727854921979470326, -227.9962554126566943 ) ) ;
#6764 =( LENGTH_UNIT ( ) NAMED_UNIT ( * ) SI_UNIT ( .MILLI., .METRE. ) );
#6765 = CARTESIAN_POINT ( 'NONE',  ( 5.133806223762193532, -16.42362916962670383, -230.4968203642818310 ) ) ;
#6766 = CARTESIAN_POINT ( 'NONE',  ( 25.30228294196351868, 7.987863777258004561, -233.0744943826964573 ) ) ;
#6767 = CARTESIAN_POINT ( 'NONE',  ( -17.08384421609436643, 23.56421365837046622, -225.2902702884460666 ) ) ;
#6768 = CARTESIAN_POINT ( 'NONE',  ( -11.23881320317003407, 15.84151802331611236, -234.2799649731619809 ) ) ;
#6769 = ORIENTED_EDGE ( 'NONE', *, *, #15276, .F. ) ;
#6770 = CARTESIAN_POINT ( 'NONE',  ( -26.10238271615538252, -1.908654064438627174, -220.4792571320490708 ) ) ;
#6771 = ORIENTED_EDGE ( 'NONE', *, *, #6721, .F. ) ;
#6772 = CARTESIAN_POINT ( 'NONE',  ( 7.743212835174657194, 11.90778931056080481, -226.0491028376908105 ) ) ;
#6773 = CARTESIAN_POINT ( 'NONE',  ( -15.60078324628501356, 3.527872497691606934, -227.4630248446626695 ) ) ;
#6774 = CARTESIAN_POINT ( 'NONE',  ( 29.64577750251057608, 2.839131411071813549, -220.9704389295326905 ) ) ;
#6775 = CARTESIAN_POINT ( 'NONE',  ( 25.50000000000000000, 0.000000000000000000, 0.000000000000000000 ) ) ;
#6776 = CARTESIAN_POINT ( 'NONE',  ( 14.60728983664449387, 19.38727400458104455, -216.6381802409380555 ) ) ;
#6777 = CARTESIAN_POINT ( 'NONE',  ( -15.65611835717891687, 5.486779671999271635, -227.0554626315911264 ) ) ;
#6778 = CARTESIAN_POINT ( 'NONE',  ( -0.9851030586975465519, 19.34066537597387381, -233.8273485600932418 ) ) ;
#6779 = CARTESIAN_POINT ( 'NONE',  ( 17.66865342763861690, 2.849170916951684784, -230.9175656266857004 ) ) ;
#6780 = CARTESIAN_POINT ( 'NONE',  ( -13.37406041957185110, -11.77244451953823834, -233.9958171493936732 ) ) ;
#6781 = ORIENTED_EDGE ( 'NONE', *, *, #12124, .T. ) ;
#6782 = CARTESIAN_POINT ( 'NONE',  ( -12.50828242918857036, -25.45147276965577277, -228.7626325223041022 ) ) ;
#6783 = TOROIDAL_SURFACE ( 'NONE', #8220, 22.63401512838748175, 3.000000000000002665 ) ;
#6784 = CARTESIAN_POINT ( 'NONE',  ( -15.42311360645077301, 11.97619046995196079, -234.9244673706848801 ) ) ;
#6785 = CARTESIAN_POINT ( 'NONE',  ( 1.780803752597676537, -13.83832444325970101, -229.2250779460899537 ) ) ;
#6786 = CARTESIAN_POINT ( 'NONE',  ( 0.4042326456706432647, 15.50845657815858303, -219.2680337625893401 ) ) ;
#6787 = CARTESIAN_POINT ( 'NONE',  ( 26.45187990207246997, -15.96729416691344383, -220.4105496189887674 ) ) ;
#6788 = CARTESIAN_POINT ( 'NONE',  ( -15.51091956967506391, -1.782849713491490018, -228.8089183834494520 ) ) ;
#6789 = EDGE_CURVE ( 'NONE', #497, #10628, #2364, .T. ) ;
#6790 = CARTESIAN_POINT ( 'NONE',  ( 13.88312867625433711, 12.44451767566605760, -217.7066242262208391 ) ) ;
#6791 = CARTESIAN_POINT ( 'NONE',  ( 1.665334536937734811E-13, -23.00000000000000355, 75.00000000000000000 ) ) ;
#6792 = CARTESIAN_POINT ( 'NONE',  ( -11.11821474075380678, 16.53100589793018926, -232.3736596382188395 ) ) ;
#6793 = CARTESIAN_POINT ( 'NONE',  ( 24.20411255886326529, 12.66254860825103634, -218.0144359054998802 ) ) ;
#6794 = CARTESIAN_POINT ( 'NONE',  ( 13.43730899468209294, 8.427513769504761498, -221.4030804848920297 ) ) ;
#6795 = CARTESIAN_POINT ( 'NONE',  ( 12.23475091788960434, 6.342242864926500800, -221.9572581868331156 ) ) ;
#6796 = CARTESIAN_POINT ( 'NONE',  ( 4.433847066018189231, -14.70588125837090487, -232.6468564462760469 ) ) ;
#6797 = CARTESIAN_POINT ( 'NONE',  ( -1.884624261322229266, 13.00421381464247084, -226.7648460381863345 ) ) ;
#6798 = MANIFOLD_SOLID_BREP ( 'Cut-Extrude-Thin1', #21569 ) ;
#6799 = CARTESIAN_POINT ( 'NONE',  ( 28.51464931495100785, 5.422321182929326966, -223.8116416110474347 ) ) ;
#6800 = CARTESIAN_POINT ( 'NONE',  ( 3.568716337251232051, -21.91366830329386772, -233.6537821856145172 ) ) ;
#6801 = CARTESIAN_POINT ( 'NONE',  ( -11.35482716595652875, 11.86850131893102223, -220.6599844941370350 ) ) ;
#6802 = EDGE_CURVE ( 'NONE', #7254, #19351, #5472, .T. ) ;
#6803 = CARTESIAN_POINT ( 'NONE',  ( 2.471164685565028662, 14.01327037412690935, -223.4905256513065410 ) ) ;
#6804 = CARTESIAN_POINT ( 'NONE',  ( -25.10035252441274167, -15.33546242866430198, -228.3913311683031964 ) ) ;
#6805 = CARTESIAN_POINT ( 'NONE',  ( 12.93042813863272755, 0.4488092930645843914, -225.5263188864764174 ) ) ;
#6806 = EDGE_CURVE ( 'NONE', #6505, #9492, #8981, .T. ) ;
#6807 = CARTESIAN_POINT ( 'NONE',  ( 21.14441169763230732, 12.98245189690719315, -217.0976687089155064 ) ) ;
#6808 = EDGE_LOOP ( 'NONE', ( #17981, #3578, #4262, #6142 ) ) ;
#6809 = CARTESIAN_POINT ( 'NONE',  ( 12.04687593227112430, 27.54339840196571743, -224.6466266724203820 ) ) ;
#6810 = CARTESIAN_POINT ( 'NONE',  ( 13.37416304104233333, -8.359606308866407431, -226.7674924273047452 ) ) ;
#6811 = CARTESIAN_POINT ( 'NONE',  ( 12.74640035234706659, -6.767230903810586895, -221.4971111014800726 ) ) ;
#6812 = FILL_AREA_STYLE ('',( #12099 ) ) ;
#6813 = CARTESIAN_POINT ( 'NONE',  ( 1.773982976645536835, 19.12448993322812285, -233.2315972735944172 ) ) ;
#6814 = CARTESIAN_POINT ( 'NONE',  ( -12.42228566111607968, -8.873047627549107474, -232.6540845750675999 ) ) ;
#6815 = CARTESIAN_POINT ( 'NONE',  ( -15.46269062504165781, -26.67469327287815517, -225.2085449711190677 ) ) ;
#6816 = CARTESIAN_POINT ( 'NONE',  ( 6.053458391837899910, -12.85229775019162268, -220.9645494416007523 ) ) ;
#6817 = CARTESIAN_POINT ( 'NONE',  ( -13.40354389326479456, 23.35336998323175450, -219.8517474526506987 ) ) ;
#6818 = CARTESIAN_POINT ( 'NONE',  ( 10.89019654021101857, 23.08162452736882031, -220.1893104909416934 ) ) ;
#6819 = CARTESIAN_POINT ( 'NONE',  ( -14.07917727715460821, 7.534853284453274291, -218.6337090155677458 ) ) ;
#6820 = CARTESIAN_POINT ( 'NONE',  ( -13.33011381921379090, 5.829915729572584304, -219.4453182727427816 ) ) ;
#6821 = CARTESIAN_POINT ( 'NONE',  ( -19.48378335617362112, -12.36282430725977655, -218.8185104403611945 ) ) ;
#6822 = ORIENTED_EDGE ( 'NONE', *, *, #4639, .F. ) ;
#6823 = CARTESIAN_POINT ( 'NONE',  ( -4.691002462566371101, 21.98518063340150164, -232.2516024630330094 ) ) ;
#6824 = CARTESIAN_POINT ( 'NONE',  ( 23.44028133050380802, 19.87677100428751231, -223.1503774981096342 ) ) ;
#6825 = CARTESIAN_POINT ( 'NONE',  ( 15.79748369401691122, 19.19631269170049137, -215.0096632418193963 ) ) ;
#6826 = CARTESIAN_POINT ( 'NONE',  ( 11.63416633096549369, -11.60453582225250990, -230.7583135875248104 ) ) ;
#6828 = EDGE_CURVE ( 'NONE', #8028, #3240, #14260, .T. ) ;
#6827 = CARTESIAN_POINT ( 'NONE',  ( 0.000000000000000000, 0.000000000000000000, 77.51594804401857175 ) ) ;
#6829 = ORIENTED_EDGE ( 'NONE', *, *, #5250, .T. ) ;
#6830 = CARTESIAN_POINT ( 'NONE',  ( -11.26857159993117996, 28.96895336474501192, -225.6039696848669678 ) ) ;
#6831 = CARTESIAN_POINT ( 'NONE',  ( -11.10256751292636324, -5.696117445562730808, -228.9287437256430451 ) ) ;
#6832 = LINE ( 'NONE', #20535, #21975 ) ;
#6833 = CARTESIAN_POINT ( 'NONE',  ( 19.19288224840068935, 10.13059690604263174, -232.1906135022504998 ) ) ;
#6834 = CARTESIAN_POINT ( 'NONE',  ( -29.30406754532526037, 5.063969254119831120, -221.8212091093853076 ) ) ;
#6835 = CARTESIAN_POINT ( 'NONE',  ( 13.49882595795384255, -9.201056071450322449, -219.2439763087855908 ) ) ;
#6836 = CARTESIAN_POINT ( 'NONE',  ( -11.46843428684449151, 6.508406145394057596, -225.7212143570321814 ) ) ;
#6837 = MANIFOLD_SOLID_BREP ( 'Mirror2', #8293 ) ;
#6838 = CARTESIAN_POINT ( 'NONE',  ( -21.89482327431018760, 1.733733432562314158, -233.1353281693111796 ) ) ;
#6839 = CARTESIAN_POINT ( 'NONE',  ( -3.515149843921121509, -20.22121776728782550, -231.9652171757311123 ) ) ;
#6840 = DIRECTION ( 'NONE',  ( -1.000000000000000000, -6.982962677686266711E-15, 0.000000000000000000 ) ) ;
#6841 = FACE_OUTER_BOUND ( 'NONE', #1862, .T. ) ;
#6842 = LINE ( 'NONE', #11681, #9140 ) ;
#6843 = CARTESIAN_POINT ( 'NONE',  ( 13.30832375548903990, -9.333840824262514602, -222.9696809959601183 ) ) ;
#6844 = CARTESIAN_POINT ( 'NONE',  ( -27.09167109716269550, -0.2825935922571593539, -219.8389404328913486 ) ) ;
#6845 = CARTESIAN_POINT ( 'NONE',  ( -21.01246475424954596, -9.353905080905251523, 3.551468768066980530 ) ) ;
#6846 = CARTESIAN_POINT ( 'NONE',  ( 14.78510113471881304, 14.77128235908076803, -230.8056908117964383 ) ) ;
#6847 = CARTESIAN_POINT ( 'NONE',  ( 10.12648780932046755, 24.76571117977573522, -228.8499436907259792 ) ) ;
#6848 = CARTESIAN_POINT ( 'NONE',  ( 7.445043070300236820, -12.68569377707410339, -219.2962123921901991 ) ) ;
#6849 = CARTESIAN_POINT ( 'NONE',  ( 5.953549895739506326, -12.70069413479034104, -221.3143591192976203 ) ) ;
#6850 = ORIENTED_EDGE ( 'NONE', *, *, #2389, .T. ) ;
#6851 = APPLICATION_CONTEXT ( 'automotive_design' ) ;
#6852 = CARTESIAN_POINT ( 'NONE',  ( -7.284474494690100776, 13.60812129561547046, -227.7414351104868331 ) ) ;
#6853 = CARTESIAN_POINT ( 'NONE',  ( -16.54465188417290022, 6.134005835925411709, -228.8256222654843270 ) ) ;
#6854 = CARTESIAN_POINT ( 'NONE',  ( 27.94758519801750296, 7.894658480667867018, -227.3974864124137127 ) ) ;
#6855 = CARTESIAN_POINT ( 'NONE',  ( -3.424870747449708652, -17.07003249573819659, -220.0803597572327135 ) ) ;
#6856 = CARTESIAN_POINT ( 'NONE',  ( -7.678935899902896267, -7.549707216296320134, 92.00000000000001421 ) ) ;
#6857 = EDGE_LOOP ( 'NONE', ( #794, #10365, #5711, #21919, #3704, #18021, #2327, #8058, #16491, #3166, #6781, #13498, #14756, #604, #16989, #13651, #2245, #9125, #12057, #10515, #278, #7371, #185, #1474, #5780, #13904 ) ) ;
#6858 = CARTESIAN_POINT ( 'NONE',  ( 21.18605525173251891, 3.426801613781890854, -232.1183243183448894 ) ) ;
#6859 = CARTESIAN_POINT ( 'NONE',  ( 12.31709745011784740, -23.08055702692190891, -220.7960250479738136 ) ) ;
#6860 = CARTESIAN_POINT ( 'NONE',  ( 4.883314309504700468, 19.06839645569368358, -217.0171359871271193 ) ) ;
#6861 = CARTESIAN_POINT ( 'NONE',  ( -15.48255455842386219, 10.01793346089237069, -233.1197357361336913 ) ) ;
#6862 = CIRCLE ( 'NONE', #7937, 12.50000000000000000 ) ;
#6863 = CARTESIAN_POINT ( 'NONE',  ( 30.65249971456167799, 3.724008896938769464, -225.4815109119605552 ) ) ;
#6864 = CARTESIAN_POINT ( 'NONE',  ( -10.84997096467605182, 25.01800101807719301, -232.4518260228253155 ) ) ;
#6865 = CARTESIAN_POINT ( 'NONE',  ( 0.6349943332661940332, 10.75744069813302595, 92.00000000000002842 ) ) ;
#6866 = CARTESIAN_POINT ( 'NONE',  ( -2.270280637033633475, -14.48864307936496765, -230.4581659391201072 ) ) ;
#6867 = FACE_OUTER_BOUND ( 'NONE', #18912, .T. ) ;
#6868 = DIRECTION ( 'NONE',  ( -2.891205793294678696E-17, 0.000000000000000000, -1.000000000000000000 ) ) ;
#6869 = CARTESIAN_POINT ( 'NONE',  ( -28.42127686227592420, -0.6461176296494712812, -221.6028628238154567 ) ) ;
#6870 = CARTESIAN_POINT ( 'NONE',  ( -26.09112266552012471, 5.807188091516064077, -215.7774933166620883 ) ) ;
#6871 = CARTESIAN_POINT ( 'NONE',  ( -14.39178795515995724, -23.41959061255243313, -230.2514514786898019 ) ) ;
#6872 =( BOUNDED_SURFACE ( )  B_SPLINE_SURFACE ( 3, 3, ( 
 ( #12046, #13513, #17114, #20575, #17002, #6643, #8565, #10025, #20351, #16778, #1462, #13628, #4946, #15429, #2036, #16887, #18903, #11822, #5163, #18688, #9797, #1581, #16663, #8118, #1244, #9915, #20464, #8456, #14983, #15324, #22170, #21823, #1354, #13283, #4713, #20239, #11592, #18466, #18797, #3028, #3366, #8226, #4833, #7099, #15649, #10799, #10577, #114, #341, #8668, #17664, #7320, #6982, #15531, #13855, #12599, #17448, #20695, #446, #21028, #3478, #15979, #10356, #3922, #2017, #8897, #2235, #15763, #14075, #9115, #556, #3587, #17219, #1792, #5616, #9004, #5272, #15868, #20802, #7432, #10694, #7209, #21133, #14300, #5720, #14190, #12153, #12494, #19010, #17558, #10464, #20913, #17327, #12263, #19341, #1904, #2127, #8787, #3811, #229, #5500, #12380, #13963, #19231, #5380, #19116, #3693, #14519, #19557, #6470, #6359, #15150, #4664, #9858, #15040, #19666, #11652, #21770, #17781, #2455, #21992, #1187, #20181, #8281, #13231, #2562, #18523, #12823, #8066, #4145, #11131, #16723, #14931, #3089, #4775, #4253, #6585, #17999, #9972, #20077, #16831, #11537, #1409, #2347, #19444, #11024, #8174, #18410, #4031, #9744, #2972, #9232, #17892, #10907, #16092, #9337, #663, #7539, #1300, #14408, #16606, #21240, #5832, #769, #16197, #21881, #13339, #12710, #7648, #21352, #5946, #15591, #18957, #3197, #3533, #8514, #17388, #20636, #3424, #8842, #3639, #15708, #10413, #285, #17274, #11771, #5221, #15267, #11988, #5329, #22224, #1848, #10520, #12102, #8726, #13795, #1964, #5107, #8619, #11876, #20517, #20411, #5000, #53, #15377, #13575, #172, #6926, #13456, #7041, #13913, #20748, #13681, #12211, #15479, #18635, #18740, #20296, #17167, #19064, #4891, #10080, #18849, #16945, #6815, #1745, #3307, #10304, #1521, #8399, #22117, #6704, #10190, #17060, #1637, #21290, #2289, #5886, #10849, #11076, #5440, #12762, #7264, #17835, #9175, #4197, #5667, #610, #12322, #14134, #19612, #17943, #12438, #2507, #3753, #7485, #14457, #21080, #9385, #16247, #10746, #19289, #14354, #12545, #7379, #12653, #393, #7154, #17612, #3866, #14020, #14247, #10638, #3975, #19176, #20856, #10964, #17505, #2072, #8952, #15816, #19392, #20972, #4087, #2400, #5560, #2178, #9059, #7588, #17723, #16038, #15925, #21186, #5772, #503, #19499, #9282, #16142, #714, #5997, #6331, #21513, #936, #12976, #3055, #7814, #16577, #4526, #11510, #18273, #16690, #21407, #6217, #6440, #21739, #14570, #16358, #2834, #13204, #21851, #4744, #12870, #20151, #9716, #1158, #1270, #21625, #19824, #13092, #2727, #14900, #4409, #9945, #11291, #7920, #20049, #18162, #8034, #14784, #14679 ),
 ( #16470, #11404, #6105, #19938, #4636, #18378, #13309, #8146, #1047, #822, #2942, #15011, #9829, #11623, #18495, #7701, #19719, #4299, #9608, #11181, #18048, #2617, #9498, #10278, #21962, #16918, #15562, #8696, #22085, #20720, #13427, #17144, #1818, #8487, #142, #3614, #20382, #6675, #1720, #15351, #17034, #28, #10055, #13882, #4976, #13547, #7010, #1609, #20268, #13656, #6555, #5301, #20607, #4864, #11741, #18609, #16805, #22199, #3171, #13768, #12075, #1380, #12183, #8256, #17247, #6787, #20491, #19037, #5082, #11963, #15123, #1492, #8370, #15240, #11851, #18932, #6898, #18824, #18716, #3396, #5193, #8595, #3280, #10165, #15456, #3507, #10386, #2375, #5642, #9258, #14217, #14433, #8815, #16117, #10607, #21159, #12518, #7565, #9033, #3949, #15678, #17476, #690, #21266, #15791, #5859, #7126, #10825, #17810, #2153, #12740, #19585, #14106, #370, #17695, #15897, #10721, #16008, #3725, #10492, #20943, #7237, #17358, #17587, #13993, #7351, #258, #1935, #14327, #20829, #5410, #12293, #19146, #477, #2047, #7459, #5747, #8925, #5530, #12409, #10937, #21052, #19368, #19260, #2264, #9147, #12627, #584, #19473, #4062, #3840, #4613, #21490, #9364, #9692, #2592, #4279, #16335, #6417, #11159, #19914, #7900, #14875, #21600, #20026, #2483, #9587, #9802, #2813, #17918, #19693, #6191, #16553, #2917, #8122, #16223, #1248, #13070, #4503, #11488, #2704, #911, #16450, #6081, #18251, #7791, #13287, #14657, #11269, #1131, #12956, #11382, #18138, #18025, #8007, #21716, #21828, #4384, #19800, #6308, #14548, #13183, #21384, #18355, #16667, #1023, #4174, #14760, #14987, #11052, #798, #7678, #5974, #9475, #12851, #5058, #15535, #20356, #15212, #6762, #8231, #6871, #15101, #5168, #20467, #10139, #3032, #1796, #118, #18584, #18907, #8342, #3483, #4837, #11596, #18692, #3370, #1585, #6987, #18470, #20129, #10360, #8672, #13743, #13632, #11935, #4717, #9919, #16783, #18800, #1358, #22058, #3255, #17006, #3, #20579, #10252, #12050, #21937, #17223, #11713, #6528, #17118, #6647, #13397, #20243, #1466, #1697, #13517, #4950, #11826, #3146, #8569, #10029, #8460, #15328, #16892, #22174, #15433, #17786, #9119, #10802, #19235, #16096, #19120, #13967, #3697, #10911, #19448, #5724, #5620, #20699, #3815, #2131, #17668, #21032, #5504, #9008, #2351, #14304, #8901, #19014, #19345, #12267, #20806, #10582, #667, #5383, #7325, #17562, #2238, #15872, #7436, #12157, #10698, #4035, #12498, #5276, #7103, #450, #3927, #12604, #9236, #3591, #13859, #14195, #15983, #21137, #12385, #17452, #560, #15767, #10468, #17331, #1908, #8792, #2021, #15653, #233, #345 ),
 ( #7213, #14079, #20917, #16641, #11135, #19670, #14737, #21466, #7764, #13042, #772, #4587, #18003, #4257, #14847, #14634, #4149, #4359, #12714, #21690, #11357, #11029, #19562, #17896, #7542, #6058, #2459, #4477, #2786, #14412, #20002, #21244, #7982, #12932, #19778, #6282, #18332, #2893, #11242, #9342, #7652, #5836, #16201, #9669, #19888, #14523, #18226, #2567, #11463, #21577, #18113, #9776, #21358, #5950, #16528, #12827, #1107, #9451, #6165, #16311, #2681, #13156, #887, #9563, #16425, #1000, #7875, #1558, #13716, #15186, #18669, #21914, #8316, #8206, #15078, #10114, #18559, #1334, #10225, #16979, #18883, #8433, #13607, #18776, #1445, #15410, #3230, #21804, #6503, #3458, #4926, #1671, #12024, #15300, #6621, #22255, #16868, #11802, #13374, #22030, #20444, #22150, #6848, #8546, #13490, #10337, #20330, #20556, #6739, #5143, #5033, #11910, #8097, #3342, #17093, #1222, #14964, #6392, #13263, #20107, #4695, #3125, #11570, #18444, #20216, #4811, #11687, #3007, #10005, #9890, #16756, #5597, #12362, #10779, #15511, #322, #535, #15851, #8650, #10447, #19212, #427, #15962, #21116, #6964, #14282, #3793, #17541, #17647, #15743, #13946, #7190, #19097, #8988, #7077, #4010, #20781, #1998, #7302, #5362, #10677, #8879, #1883, #2108, #14172, #12581, #17428, #12246, #21007, #5255, #3904, #12135, #2213, #12478, #14056, #93, #5703, #19424, #15627, #7412, #3674, #17201, #8766, #13835, #20892, #19324, #5479, #1776, #20671, #18991, #3570, #17307, #9095, #207, #10558, #13130, #17762, #19975, #2655, #6255, #21330, #16286, #860, #13015, #11329, #9536, #4447, #10886, #18198, #2435, #1081, #7849, #12801, #16503, #2326, #14495, #16396, #5924, #19647, #4232, #5809, #4334, #2761, #7738, #11112, #12690, #14608, #17980, #14820, #6141, #14715, #21443, #9211, #16179, #11005, #750, #7955, #21665, #9642, #16074, #7626, #644, #6033, #7521, #14389, #11218, #12907, #21222, #2543, #19754, #17873, #9422, #21550, #18086, #19537, #4124, #975, #9319, #19861, #18746, #21998, #3313, #8287, #8520, #2866, #10198, #4670, #15273, #6593, #1643, #3095, #20302, #9750, #11543, #17066, #15383, #9864, #22230, #1195, #4897, #11883, #18529, #6821, #13687, #8181, #16729, #11777, #9978, #4783, #10086, #20083, #4562, #15046, #1306, #11438, #11658, #8072, #1415, #16613, #18307, #8406, #14937, #21777, #6365, #13237, #16839, #18417, #1527, #22123, #2980, #21887, #6476, #5006, #15156, #13462, #13345, #20187, #18641, #3204, #16951, #6710, #13581, #20417, #694, #4066, #10310, #10941, #15600, #2487, #5751, #10828, #16227, #11055, #803, #17814, #7682, #2379, #18855, #12631, #59 ),
 ( #589, #21164, #21271, #19372, #17281, #17699, #480, #19477, #10420, #20524, #1855, #5646, #9263, #8733, #7462, #12523, #5228, #3541, #20643, #7355, #17923, #4179, #12743, #16120, #5113, #3953, #9150, #7570, #14436, #2266, #16012, #9367, #5862, #14222, #3430, #19589, #18964, #12109, #21058, #11995, #14330, #17174, #1751, #8625, #15486, #6933, #13804, #19918, #20132, #13186, #5978, #7796, #9696, #20030, #13291, #18473, #4283, #11602, #16557, #14878, #14992, #13074, #11273, #4505, #16454, #6312, #4388, #1361, #18142, #21605, #4617, #2708, #1136, #6197, #21494, #8014, #21719, #9922, #14764, #9591, #11492, #2598, #1251, #9479, #21831, #18359, #11386, #19696, #3036, #16786, #12960, #4721, #1026, #14551, #6084, #12854, #18254, #2921, #2817, #21387, #11162, #18029, #16339, #915, #8126, #9808, #16671, #14660, #19804, #7903, #6420, #8673, #13519, #1588, #8463, #5, #20583, #3372, #13746, #8235, #5169, #8346, #10361, #1698, #11828, #3484, #15104, #20360, #8570, #18695, #3258, #10142, #10033, #18802, #18908, #15330, #17011, #16895, #6765, #22176, #1797, #6874, #15435, #13634, #21941, #5061, #12051, #20246, #20469, #17224, #15537, #4841, #15217, #11938, #6533, #13402, #11717, #1470, #18587, #3149, #22061, #6651, #4952, #10253, #17119, #18873, #3332, #10328, #81, #7066, #3448, #1767, #6952, #11900, #3559, #13707, #9996, #16968, #13935, #15400, #12125, #196, #5131, #17084, #10437, #5024, #22247, #18661, #10215, #8641, #6839, #17297, #18980, #18763, #20770, #1661, #1872, #20544, #8755, #12015, #15616, #16858, #11678, #11794, #13824, #17190, #18549, #8536, #15502, #1434, #3221, #3116, #8307, #1547, #15174, #22020, #20661, #6612, #5243, #13481, #20320, #15291, #8424, #4918, #10104, #22140, #6730, #13598, #20435, #8976, #17529, #12678, #12467, #1987, #2202, #10547, #19526, #9199, #8867, #17417, #15732, #14482, #19313, #309, #2314, #634, #5352, #17861, #12235, #5797, #3891, #10769, #4113, #16168, #738, #17635, #7180, #5467, #19086, #3662, #7510, #10874, #14045, #17750, #416, #9307, #12569, #9083, #7614, #2424, #20881, #16064, #12350, #19414, #19202, #15840, #15950, #525, #14377, #10992, #3998, #21211, #3782, #10664, #2096, #7290, #14161, #20997, #5587, #7403, #14273, #21105, #5690, #16384, #963, #16273, #14808, #13226, #4435, #14703, #848, #18187, #21537, #2967, #16601, #18296, #11317, #1295, #4323, #21432, #11206, #18405, #4659, #20072, #13118, #5913, #2750, #9631, #2855, #6244, #13002, #16493, #9853, #21765, #7837, #4220, #4551, #19743, #6022, #18072, #8169, #12895, #21651, #1070, #9739, #7944, #14925, #19636, #19964, #11532 ),
 ( #11427, #2644, #6128, #9524, #19848, #1182, #8060, #6354, #16718, #21316, #12790, #11100, #17968, #2532, #9409, #7726, #14597, #13334, #20291, #17268, #18735, #15475, #3527, #8509, #20406, #13790, #8394, #3301, #21987, #6698, #11983, #10185, #20628, #48, #15262, #1840, #22111, #6921, #17054, #5214, #1631, #18951, #20176, #12096, #15145, #3419, #15372, #10406, #13570, #22219, #4770, #6810, #8614, #11646, #4995, #15035, #13676, #6465, #8276, #20513, #5103, #21876, #18517, #3084, #9967, #18844, #10299, #16826, #11871, #11766, #17163, #1404, #18630, #1740, #6580, #3192, #13450, #4886, #10075, #16940, #1516, #15700, #17604, #15918, #4081, #8945, #3745, #2172, #19058, #17717, #3634, #16029, #9050, #20963, #13906, #12647, #10957, #7147, #7477, #19169, #14347, #277, #163, #7255, #14238, #12430, #17830, #7033, #8718, #21180, #19494, #2282, #496, #7370, #15585, #20741, #5322, #21073, #12203, #10629, #14127, #5551, #10842, #9166, #5661, #603, #10514, #5765, #14012, #17380, #12538, #17498, #1955, #8833, #12315, #19385, #2065, #15810, #387, #20849, #3968, #5431, #19281, #3858, #10739, #21508, #2612, #6326, #19933, #21620, #7809, #4631, #7696, #2501, #14566, #21734, #8029, #16571, #16466, #9276, #14674, #12972, #6213, #9604, #16354, #19819, #13198, #2830, #19712, #7583, #7915, #818, #9380, #21401, #11505, #16240, #18156, #6099, #13088, #4405, #1042, #1153, #20043, #14450, #2393, #11286, #2723, #9711, #931, #5992, #14779, #16136, #12866, #4520, #11399, #4295, #9493, #18267, #11176, #14895, #708, #18043, #21285, #5880, #12757, #19606, #4192, #11069, #17938, #5076, #13304, #3390, #18710, #8363, #1265, #22, #20600, #16800, #17138, #6549, #1713, #3050, #9824, #16911, #1603, #22079, #5187, #16685, #18373, #8589, #6891, #11955, #11845, #3273, #2935, #8141, #15006, #10158, #13761, #13422, #1486, #15234, #20485, #18818, #17028, #10272, #21844, #15451, #9940, #6435, #15344, #20262, #20146, #4739, #21957, #8481, #4859, #11736, #18604, #11617, #22193, #18490, #6668, #3165, #1374, #13541, #10049, #8250, #13650, #6780, #20376, #15118, #4969, #12177, #17352, #9445, #17997, #4251, #3835, #18926, #17471, #364, #9028, #19255, #3720, #7232, #881, #12821, #7120, #17241, #17582, #10485, #19031, #1929, #14629, #3608, #5525, #15786, #470, #14099, #5943, #10378, #2042, #2560, #10716, #3501, #5296, #19664, #12404, #2148, #21461, #1812, #12069, #15891, #7757, #252, #8920, #20938, #14517, #11129, #7646, #16306, #8690, #15556, #8809, #136, #21349, #13986, #7004, #13877, #15672, #20715, #20824, #5403, #12287, #19139, #10602, #20211, #11458, #21685 ),
 ( #18553, #12927, #6497, #13150, #19996, #4806, #16863, #1438, #4582, #11237, #6159, #19773, #4352, #8201, #11564, #18107, #18439, #1101, #10000, #13258, #18327, #8311, #3120, #15179, #3002, #6053, #9885, #2675, #20101, #7870, #2887, #11682, #14842, #16749, #9557, #4690, #1329, #6385, #16419, #9770, #1217, #4470, #16636, #13036, #19883, #14958, #15071, #8092, #21909, #13368, #995, #14733, #21572, #11351, #6276, #18221, #21799, #2780, #9664, #16523, #7976, #201, #10552, #15506, #5137, #20774, #15404, #10332, #6734, #13711, #18984, #17194, #5356, #7070, #22250, #8872, #6843, #13939, #1771, #12239, #3452, #3666, #20324, #19090, #22143, #10441, #20549, #5247, #8645, #1990, #13485, #22025, #17421, #6616, #15620, #86, #6957, #4922, #11798, #18665, #13829, #3225, #10219, #12019, #18877, #1876, #10108, #20665, #16973, #1552, #8428, #13602, #15295, #3563, #1665, #20439, #5028, #3337, #12129, #17088, #8540, #17301, #11904, #8760, #18769, #21109, #9086, #17534, #12574, #15955, #19640, #10996, #12682, #5694, #17972, #21001, #15844, #5591, #12794, #21322, #7618, #7514, #313, #19418, #4002, #19531, #638, #7407, #10877, #4225, #16172, #10773, #20885, #21215, #14166, #420, #12471, #2536, #7294, #9204, #17755, #4117, #2318, #9311, #14049, #16067, #5917, #14381, #7184, #8980, #5801, #17866, #14486, #11104, #5471, #15736, #2428, #742, #12355, #14277, #19317, #19205, #3786, #3896, #10668, #2100, #17639, #529, #2206, #21542, #11431, #1074, #16388, #18300, #16605, #4774, #9635, #4439, #2859, #19747, #18409, #4327, #16722, #9743, #21656, #14601, #13338, #11651, #7841, #8173, #19852, #15039, #967, #853, #4555, #2971, #7730, #14812, #21880, #8065, #21436, #2648, #1186, #14930, #6469, #20180, #6026, #18522, #21769, #6358, #9857, #7948, #6132, #6248, #9413, #13006, #13230, #20076, #11322, #16497, #4663, #18191, #11536, #13122, #14707, #1299, #16277, #12900, #19968, #2754, #11210, #18076, #9529, #20295, #10412, #3423, #15376, #8280, #7040, #5328, #1520, #1847, #13574, #8725, #10079, #16830, #1636, #8618, #6814, #12210, #1408, #3088, #15590, #13912, #18956, #18848, #10303, #9971, #15149, #21991, #17166, #20747, #20410, #8513, #22223, #5220, #3532, #1744, #17273, #6584, #171, #16944, #13455, #52, #4999, #4890, #11770, #6703, #15478, #11875, #18739, #3306, #18634, #6925, #3196, #13680, #10189, #8398, #20516, #17059, #15266, #20635, #13794, #5106, #22116, #11987, #12101, #2071, #16141, #2398, #10963, #10848, #3638, #2177, #7378, #16037, #3974, #10745, #14246, #7587, #19498, #14133, #1963, #2288, #17504, #19175, #8951, #21289, #3752, #12544 ),
 ( #8841, #9174, #20971, #713, #17722, #9058, #14456, #9281, #5885, #609, #19063, #7484, #17387, #14353, #20855, #17611, #17834, #5559, #21185, #10519, #5771, #12652, #19391, #15707, #15924, #21079, #15815, #3865, #10637, #392, #5666, #4086, #502, #284, #7153, #14019, #5439, #12321, #7263, #19288, #12437, #14782, #11074, #18047, #15010, #16469, #13203, #1269, #6216, #18161, #11509, #6103, #1046, #19717, #4408, #9715, #7919, #18377, #20048, #12975, #21850, #19823, #4635, #21624, #2941, #13091, #16689, #17942, #9828, #12869, #1157, #19937, #8145, #11290, #4525, #2506, #4298, #12761, #19611, #2616, #4196, #9384, #11403, #16246, #2726, #821, #7700, #16357, #9497, #18272, #9607, #2833, #16576, #5996, #14569, #935, #7813, #21406, #8033, #11180, #14899, #14678, #21512, #21738, #6330, #11622, #9944, #15560, #20380, #18494, #3394, #1718, #6439, #18930, #13308, #6896, #13545, #4974, #20605, #17245, #3054, #6554, #5191, #12073, #11740, #10384, #16804, #22197, #13766, #11849, #3505, #20150, #10053, #18608, #13654, #18714, #6673, #11961, #21961, #1816, #16916, #3170, #8694, #3278, #1379, #10163, #8255, #4743, #10276, #15122, #13426, #20267, #4863, #17032, #1490, #17142, #8593, #8368, #15238, #22083, #1607, #8485, #15349, #6785, #20489, #5080, #18822, #15454, #26, #7008, #20718, #2262, #5640, #12181, #12516, #17474, #4060, #7349, #12407, #17808, #12625, #2373, #19366, #9256, #3947, #5299, #14215, #1933, #20941, #14325, #8923, #10823, #19471, #21050, #17693, #475, #10935, #14104, #17585, #20827, #7235, #7124, #13991, #9031, #9145, #5528, #16006, #582, #140, #7457, #21157, #5745, #368, #13880, #2151, #19035, #5408, #3612, #3838, #10490, #17356, #15895, #19258, #8813, #15789, #10719, #12291, #15676, #256, #19143, #3723, #10605, #2045, #2915, #9473, #8005, #11267, #14873, #19798, #20024, #14431, #21714, #16221, #4501, #18136, #13181, #14655, #9585, #14546, #796, #5972, #18353, #7676, #16448, #4382, #11380, #2702, #9690, #21264, #21488, #6306, #14758, #7563, #9362, #1021, #21598, #4611, #11486, #5857, #16115, #7898, #6189, #16551, #6079, #12849, #12954, #688, #19691, #13068, #19912, #4277, #909, #18249, #11157, #2811, #7789, #21382, #1129, #12738, #19583, #16333, #18023, #4172, #11050, #17916, #2480, #2590, #10137, #22056, #14985, #13740, #12048, #8229, #8567, #20241, #15431, #16781, #1246, #8340, #15326, #13515, #18905, #8120, #9799, #1, #20577, #3368, #3253, #17004, #16665, #21826, #6415, #1583, #5166, #4835, #15210, #6645, #11933, #10250, #8458, #17116, #13285, #1695, #1356, #6869, #6760, #11711, #20127, #4715, #13395 ) ),
 .UNSPECIFIED., .T., .F., .F. ) 
 B_SPLINE_SURFACE_WITH_KNOTS ( ( 4, 3, 4 ),
 ( 4, 2, 2, 2, 2, 2, 2, 2, 2, 2, 2, 2, 2, 2, 2, 2, 2, 2, 2, 2, 2, 2, 2, 2, 2, 2, 2, 2, 2, 2, 2, 2, 2, 2, 2, 2, 2, 2, 2, 2, 2, 2, 2, 2, 2, 2, 2, 2, 2, 2, 2, 2, 2, 2, 2, 2, 2, 2, 2, 2, 2, 2, 2, 2, 2, 2, 2, 2, 2, 2, 2, 2, 2, 2, 2, 2, 2, 2, 2, 2, 2, 2, 2, 2, 2, 2, 2, 2, 2, 2, 2, 2, 2, 2, 2, 2, 2, 2, 2, 2, 2, 2, 2, 2, 2, 2, 2, 2, 2, 2, 2, 2, 2, 2, 2, 2, 2, 2, 2, 2, 2, 2, 2, 2, 2, 2, 2, 2, 2, 2, 2, 2, 2, 2, 2, 2, 2, 2, 2, 2, 2, 2, 2, 2, 2, 2, 2, 2, 2, 2, 2, 2, 2, 2, 2, 2, 2, 2, 2, 2, 2, 2, 2, 2, 2, 2, 2, 2, 2, 4 ),
 ( 0.000000000000000000, 0.5000000000000000000, 1.000000000000000000 ),
 ( 0.4999446919652688059, 0.5028747035357847839, 0.5058047151063008728, 0.5087347266768169618, 0.5116647382473329397, 0.5145947498178489177, 0.5175247613883648956, 0.5204547729588808735, 0.5233847845293969625, 0.5268031313616656774, 0.5285123047777999794, 0.5302214781939342814, 0.5336398250262029963, 0.5353489984423374093, 0.5370581718584717112, 0.5404765186907403152, 0.5438948655230090301, 0.5473132123552777450, 0.5507315591875463490, 0.5541499060198149529, 0.5575682528520836678, 0.5609865996843523828, 0.5644049465166209867, 0.5661141199327552886, 0.5678232933488895906, 0.5712416401811581945, 0.5729508135972924965, 0.5746599870134267984, 0.5780783338456955134, 0.5814966806779642283, 0.5849150275102328322, 0.5883333743425015472, 0.5917517211747702621, 0.5951700680070388660, 0.5985884148393075810, 0.6020067616715762959, 0.6037159350877105979, 0.6054251085038448998, 0.6088434553361135038, 0.6122618021683822187, 0.6139709755845166317, 0.6156801490006509336, 0.6190984958329195376, 0.6225168426651882525, 0.6259351894974569674, 0.6293535363297255714, 0.6327718831619942863, 0.6361902299942630012, 0.6396085768265316052, 0.6430269236588003201, 0.6447360970749347331, 0.6464452704910690350, 0.6498636173233376390, 0.6532819641556063539, 0.6549911375717407669, 0.6567003109878750688, 0.6601186578201436728, 0.6635370046524122767, 0.6669553514846809916, 0.6703736983169497066, 0.6737920451492183105, 0.6772103919814870254, 0.6806287388137557404, 0.6840470856460243443, 0.6857562590621586462, 0.6866108457702257972, 0.6874654324782930592, 0.6908837793105617742, 0.6943021261428303781, 0.6960112995589646800, 0.6977204729750989820, 0.7011388198073676969, 0.7045571666396364119, 0.7079755134719050158, 0.7113938603041736197, 0.7148122071364423347, 0.7182305539687110496, 0.7216489008009796535, 0.7250672476332483685, 0.7267764210493827814, 0.7284855944655170834, 0.7319039412977856873, 0.7353222881300544023, 0.7387406349623231172, 0.7421589817945917211, 0.7455773286268603250, 0.7489956754591290400, 0.7524140222913977549, 0.7558323691236663588, 0.7592507159559350738, 0.7626690627882037887, 0.7660874096204723926, 0.7695057564527411076, 0.7729241032850098225, 0.7763424501172784264, 0.7797607969495471414, 0.7831791437818158563, 0.7865974906140844602, 0.7900158374463531752, 0.7934341842786218901, 0.7968525311108904940, 0.8002708779431590980, 0.8036892247754278129, 0.8053983981915622259, 0.8071075716076965278, 0.8105259184399651318, 0.8122350918560994337, 0.8139442652722337357, 0.8173626121045024506, 0.8207809589367711656, 0.8241993057690397695, 0.8276176526013083734, 0.8310359994335770883, 0.8344543462658458033, 0.8378726930981144072, 0.8412910399303831221, 0.8430002133465175351, 0.8447093867626518371, 0.8481277335949204410, 0.8515460804271891559, 0.8549644272594578709, 0.8583827740917264748, 0.8618011209239951897, 0.8652194677562639047, 0.8686378145885325086, 0.8720561614208012235, 0.8754745082530699385, 0.8788928550853385424, 0.8823112019176071463, 0.8857295487498758613, 0.8874387221660102743, 0.8891478955821445762, 0.8925662424144131801, 0.8942754158305474821, 0.8959845892466818951, 0.8994029360789506100, 0.9028212829112192139, 0.9062396297434879289, 0.9096579765757566438, 0.9130763234080252477, 0.9164946702402939627, 0.9199130170725626776, 0.9233313639048312815, 0.9250405373209655835, 0.9267497107370999965, 0.9301680575693687114, 0.9335864044016373153, 0.9352955778177716173, 0.9370047512339059192, 0.9404230980661746342, 0.9438414448984433491, 0.9472597917307119531, 0.9506781385629806680, 0.9540964853952493829, 0.9575148322275179869, 0.9609331790597867018, 0.9643515258920554167, 0.9660606993081897187, 0.9677698727243240207, 0.9711882195565927356, 0.9728973929727271486, 0.9746065663888614505, 0.9780249132211300545, 0.9814432600533987694, 0.9848616068856674843, 0.9882799537179360883, 0.9912099652884520662, 0.9941399768589680441, 0.9970699884294840221, 1.000000000000000000 ),
 .UNSPECIFIED. ) 
 GEOMETRIC_REPRESENTATION_ITEM ( )  RATIONAL_B_SPLINE_SURFACE ( (
 ( 1.000000000000000000, 1.000000000000000000, 1.000000000000000000, 1.000000000000000000, 1.000000000000000000, 1.000000000000000000, 1.000000000000000000, 1.000000000000000000, 1.000000000000000000, 1.000000000000000000, 1.000000000000000000, 1.000000000000000000, 1.000000000000000000, 1.000000000000000000, 1.000000000000000000, 1.000000000000000000, 1.000000000000000000, 1.000000000000000000, 1.000000000000000000, 1.000000000000000000, 1.000000000000000000, 1.000000000000000000, 1.000000000000000000, 1.000000000000000000, 1.000000000000000000, 1.000000000000000000, 1.000000000000000000, 1.000000000000000000, 1.000000000000000000, 1.000000000000000000, 1.000000000000000000, 1.000000000000000000, 1.000000000000000000, 1.000000000000000000, 1.000000000000000000, 1.000000000000000000, 1.000000000000000000, 1.000000000000000000, 1.000000000000000000, 1.000000000000000000, 1.000000000000000000, 1.000000000000000000, 1.000000000000000000, 1.000000000000000000, 1.000000000000000000, 1.000000000000000000, 1.000000000000000000, 1.000000000000000000, 1.000000000000000000, 1.000000000000000000, 1.000000000000000000, 1.000000000000000000, 1.000000000000000000, 1.000000000000000000, 1.000000000000000000, 1.000000000000000000, 1.000000000000000000, 1.000000000000000000, 1.000000000000000000, 1.000000000000000000, 1.000000000000000000, 1.000000000000000000, 1.000000000000000000, 1.000000000000000000, 1.000000000000000000, 1.000000000000000000, 1.000000000000000000, 1.000000000000000000, 1.000000000000000000, 1.000000000000000000, 1.000000000000000000, 1.000000000000000000, 1.000000000000000000, 1.000000000000000000, 1.000000000000000000, 1.000000000000000000, 1.000000000000000000, 1.000000000000000000, 1.000000000000000000, 1.000000000000000000, 1.000000000000000000, 1.000000000000000000, 1.000000000000000000, 1.000000000000000000, 1.000000000000000000, 1.000000000000000000, 1.000000000000000000, 1.000000000000000000, 1.000000000000000000, 1.000000000000000000, 1.000000000000000000, 1.000000000000000000, 1.000000000000000000, 1.000000000000000000, 1.000000000000000000, 1.000000000000000000, 1.000000000000000000, 1.000000000000000000, 1.000000000000000000, 1.000000000000000000, 1.000000000000000000, 1.000000000000000000, 1.000000000000000000, 1.000000000000000000, 1.000000000000000000, 1.000000000000000000, 1.000000000000000000, 1.000000000000000000, 1.000000000000000000, 1.000000000000000000, 1.000000000000000000, 1.000000000000000000, 1.000000000000000000, 1.000000000000000000, 1.000000000000000000, 1.000000000000000000, 1.000000000000000000, 1.000000000000000000, 1.000000000000000000, 1.000000000000000000, 1.000000000000000000, 1.000000000000000000, 1.000000000000000000, 1.000000000000000000, 1.000000000000000000, 1.000000000000000000, 1.000000000000000000, 1.000000000000000000, 1.000000000000000000, 1.000000000000000000, 1.000000000000000000, 1.000000000000000000, 1.000000000000000000, 1.000000000000000000, 1.000000000000000000, 1.000000000000000000, 1.000000000000000000, 1.000000000000000000, 1.000000000000000000, 1.000000000000000000, 1.000000000000000000, 1.000000000000000000, 1.000000000000000000, 1.000000000000000000, 1.000000000000000000, 1.000000000000000000, 1.000000000000000000, 1.000000000000000000, 1.000000000000000000, 1.000000000000000000, 1.000000000000000000, 1.000000000000000000, 1.000000000000000000, 1.000000000000000000, 1.000000000000000000, 1.000000000000000000, 1.000000000000000000, 1.000000000000000000, 1.000000000000000000, 1.000000000000000000, 1.000000000000000000, 1.000000000000000000, 1.000000000000000000, 1.000000000000000000, 1.000000000000000000, 1.000000000000000000, 1.000000000000000000, 1.000000000000000000, 1.000000000000000000, 1.000000000000000000, 1.000000000000000000, 1.000000000000000000, 1.000000000000000000, 1.000000000000000000, 1.000000000000000000, 1.000000000000000000, 1.000000000000000000, 1.000000000000000000, 1.000000000000000000, 1.000000000000000000, 1.000000000000000000, 1.000000000000000000, 1.000000000000000000, 1.000000000000000000, 1.000000000000000000, 1.000000000000000000, 1.000000000000000000, 1.000000000000000000, 1.000000000000000000, 1.000000000000000000, 1.000000000000000000, 1.000000000000000000, 1.000000000000000000, 1.000000000000000000, 1.000000000000000000, 1.000000000000000000, 1.000000000000000000, 1.000000000000000000, 1.000000000000000000, 1.000000000000000000, 1.000000000000000000, 1.000000000000000000, 1.000000000000000000, 1.000000000000000000, 1.000000000000000000, 1.000000000000000000, 1.000000000000000000, 1.000000000000000000, 1.000000000000000000, 1.000000000000000000, 1.000000000000000000, 1.000000000000000000, 1.000000000000000000, 1.000000000000000000, 1.000000000000000000, 1.000000000000000000, 1.000000000000000000, 1.000000000000000000, 1.000000000000000000, 1.000000000000000000, 1.000000000000000000, 1.000000000000000000, 1.000000000000000000, 1.000000000000000000, 1.000000000000000000, 1.000000000000000000, 1.000000000000000000, 1.000000000000000000, 1.000000000000000000, 1.000000000000000000, 1.000000000000000000, 1.000000000000000000, 1.000000000000000000, 1.000000000000000000, 1.000000000000000000, 1.000000000000000000, 1.000000000000000000, 1.000000000000000000, 1.000000000000000000, 1.000000000000000000, 1.000000000000000000, 1.000000000000000000, 1.000000000000000000, 1.000000000000000000, 1.000000000000000000, 1.000000000000000000, 1.000000000000000000, 1.000000000000000000, 1.000000000000000000, 1.000000000000000000, 1.000000000000000000, 1.000000000000000000, 1.000000000000000000, 1.000000000000000000, 1.000000000000000000, 1.000000000000000000, 1.000000000000000000, 1.000000000000000000, 1.000000000000000000, 1.000000000000000000, 1.000000000000000000, 1.000000000000000000, 1.000000000000000000, 1.000000000000000000, 1.000000000000000000, 1.000000000000000000, 1.000000000000000000, 1.000000000000000000, 1.000000000000000000, 1.000000000000000000, 1.000000000000000000, 1.000000000000000000, 1.000000000000000000, 1.000000000000000000, 1.000000000000000000, 1.000000000000000000, 1.000000000000000000, 1.000000000000000000, 1.000000000000000000, 1.000000000000000000, 1.000000000000000000, 1.000000000000000000, 1.000000000000000000, 1.000000000000000000, 1.000000000000000000, 1.000000000000000000, 1.000000000000000000, 1.000000000000000000, 1.000000000000000000, 1.000000000000000000, 1.000000000000000000, 1.000000000000000000, 1.000000000000000000, 1.000000000000000000, 1.000000000000000000, 1.000000000000000000, 1.000000000000000000, 1.000000000000000000, 1.000000000000000000, 1.000000000000000000, 1.000000000000000000, 1.000000000000000000, 1.000000000000000000, 1.000000000000000000, 1.000000000000000000, 1.000000000000000000, 1.000000000000000000, 1.000000000000000000, 1.000000000000000000, 1.000000000000000000, 1.000000000000000000, 1.000000000000000000, 1.000000000000000000, 1.000000000000000000, 1.000000000000000000, 1.000000000000000000, 1.000000000000000000, 1.000000000000000000, 1.000000000000000000, 1.000000000000000000, 1.000000000000000000, 1.000000000000000000, 1.000000000000000000, 1.000000000000000000, 1.000000000000000000, 1.000000000000000000, 1.000000000000000000, 1.000000000000000000, 1.000000000000000000, 1.000000000000000000, 1.000000000000000000, 1.000000000000000000, 1.000000000000000000, 1.000000000000000000, 1.000000000000000000, 1.000000000000000000, 1.000000000000000000, 1.000000000000000000, 1.000000000000000000, 1.000000000000000000),
 ( 0.3333333333333333703, 0.3333333333333333703, 0.3333333333333333703, 0.3333333333333333703, 0.3333333333333333703, 0.3333333333333333703, 0.3333333333333333703, 0.3333333333333333703, 0.3333333333333333703, 0.3333333333333333703, 0.3333333333333333703, 0.3333333333333333703, 0.3333333333333333703, 0.3333333333333333703, 0.3333333333333333703, 0.3333333333333333703, 0.3333333333333333703, 0.3333333333333333703, 0.3333333333333333703, 0.3333333333333333703, 0.3333333333333333703, 0.3333333333333333703, 0.3333333333333333703, 0.3333333333333333703, 0.3333333333333333703, 0.3333333333333333703, 0.3333333333333333703, 0.3333333333333333703, 0.3333333333333333703, 0.3333333333333333703, 0.3333333333333333703, 0.3333333333333333703, 0.3333333333333333703, 0.3333333333333333703, 0.3333333333333333703, 0.3333333333333333703, 0.3333333333333333703, 0.3333333333333333703, 0.3333333333333333703, 0.3333333333333333703, 0.3333333333333333703, 0.3333333333333333703, 0.3333333333333333703, 0.3333333333333333703, 0.3333333333333333703, 0.3333333333333333703, 0.3333333333333333703, 0.3333333333333333703, 0.3333333333333333703, 0.3333333333333333703, 0.3333333333333333703, 0.3333333333333333703, 0.3333333333333333703, 0.3333333333333333703, 0.3333333333333333703, 0.3333333333333333703, 0.3333333333333333703, 0.3333333333333333703, 0.3333333333333333703, 0.3333333333333333703, 0.3333333333333333703, 0.3333333333333333703, 0.3333333333333333703, 0.3333333333333333703, 0.3333333333333333703, 0.3333333333333333703, 0.3333333333333333703, 0.3333333333333333703, 0.3333333333333333703, 0.3333333333333333703, 0.3333333333333333703, 0.3333333333333333703, 0.3333333333333333703, 0.3333333333333333703, 0.3333333333333333703, 0.3333333333333333703, 0.3333333333333333703, 0.3333333333333333703, 0.3333333333333333703, 0.3333333333333333703, 0.3333333333333333703, 0.3333333333333333703, 0.3333333333333333703, 0.3333333333333333703, 0.3333333333333333703, 0.3333333333333333703, 0.3333333333333333703, 0.3333333333333333703, 0.3333333333333333703, 0.3333333333333333703, 0.3333333333333333703, 0.3333333333333333703, 0.3333333333333333703, 0.3333333333333333703, 0.3333333333333333703, 0.3333333333333333703, 0.3333333333333333703, 0.3333333333333333703, 0.3333333333333333703, 0.3333333333333333703, 0.3333333333333333703, 0.3333333333333333703, 0.3333333333333333703, 0.3333333333333333703, 0.3333333333333333703, 0.3333333333333333703, 0.3333333333333333703, 0.3333333333333333703, 0.3333333333333333703, 0.3333333333333333703, 0.3333333333333333703, 0.3333333333333333703, 0.3333333333333333703, 0.3333333333333333703, 0.3333333333333333703, 0.3333333333333333703, 0.3333333333333333703, 0.3333333333333333703, 0.3333333333333333703, 0.3333333333333333703, 0.3333333333333333703, 0.3333333333333333703, 0.3333333333333333703, 0.3333333333333333703, 0.3333333333333333703, 0.3333333333333333703, 0.3333333333333333703, 0.3333333333333333703, 0.3333333333333333703, 0.3333333333333333703, 0.3333333333333333703, 0.3333333333333333703, 0.3333333333333333703, 0.3333333333333333703, 0.3333333333333333703, 0.3333333333333333703, 0.3333333333333333703, 0.3333333333333333703, 0.3333333333333333703, 0.3333333333333333703, 0.3333333333333333703, 0.3333333333333333703, 0.3333333333333333703, 0.3333333333333333703, 0.3333333333333333703, 0.3333333333333333703, 0.3333333333333333703, 0.3333333333333333703, 0.3333333333333333703, 0.3333333333333333703, 0.3333333333333333703, 0.3333333333333333703, 0.3333333333333333703, 0.3333333333333333703, 0.3333333333333333703, 0.3333333333333333703, 0.3333333333333333703, 0.3333333333333333703, 0.3333333333333333703, 0.3333333333333333703, 0.3333333333333333703, 0.3333333333333333703, 0.3333333333333333703, 0.3333333333333333703, 0.3333333333333333703, 0.3333333333333333703, 0.3333333333333333703, 0.3333333333333333703, 0.3333333333333333703, 0.3333333333333333703, 0.3333333333333333703, 0.3333333333333333703, 0.3333333333333333703, 0.3333333333333333703, 0.3333333333333333703, 0.3333333333333333703, 0.3333333333333333703, 0.3333333333333333703, 0.3333333333333333703, 0.3333333333333333703, 0.3333333333333333703, 0.3333333333333333703, 0.3333333333333333703, 0.3333333333333333703, 0.3333333333333333703, 0.3333333333333333703, 0.3333333333333333703, 0.3333333333333333703, 0.3333333333333333703, 0.3333333333333333703, 0.3333333333333333703, 0.3333333333333333703, 0.3333333333333333703, 0.3333333333333333703, 0.3333333333333333703, 0.3333333333333333703, 0.3333333333333333703, 0.3333333333333333703, 0.3333333333333333703, 0.3333333333333333703, 0.3333333333333333703, 0.3333333333333333703, 0.3333333333333333703, 0.3333333333333333703, 0.3333333333333333703, 0.3333333333333333703, 0.3333333333333333703, 0.3333333333333333703, 0.3333333333333333703, 0.3333333333333333703, 0.3333333333333333703, 0.3333333333333333703, 0.3333333333333333703, 0.3333333333333333703, 0.3333333333333333703, 0.3333333333333333703, 0.3333333333333333703, 0.3333333333333333703, 0.3333333333333333703, 0.3333333333333333703, 0.3333333333333333703, 0.3333333333333333703, 0.3333333333333333703, 0.3333333333333333703, 0.3333333333333333703, 0.3333333333333333703, 0.3333333333333333703, 0.3333333333333333703, 0.3333333333333333703, 0.3333333333333333703, 0.3333333333333333703, 0.3333333333333333703, 0.3333333333333333703, 0.3333333333333333703, 0.3333333333333333703, 0.3333333333333333703, 0.3333333333333333703, 0.3333333333333333703, 0.3333333333333333703, 0.3333333333333333703, 0.3333333333333333703, 0.3333333333333333703, 0.3333333333333333703, 0.3333333333333333703, 0.3333333333333333703, 0.3333333333333333703, 0.3333333333333333703, 0.3333333333333333703, 0.3333333333333333703, 0.3333333333333333703, 0.3333333333333333703, 0.3333333333333333703, 0.3333333333333333703, 0.3333333333333333703, 0.3333333333333333703, 0.3333333333333333703, 0.3333333333333333703, 0.3333333333333333703, 0.3333333333333333703, 0.3333333333333333703, 0.3333333333333333703, 0.3333333333333333703, 0.3333333333333333703, 0.3333333333333333703, 0.3333333333333333703, 0.3333333333333333703, 0.3333333333333333703, 0.3333333333333333703, 0.3333333333333333703, 0.3333333333333333703, 0.3333333333333333703, 0.3333333333333333703, 0.3333333333333333703, 0.3333333333333333703, 0.3333333333333333703, 0.3333333333333333703, 0.3333333333333333703, 0.3333333333333333703, 0.3333333333333333703, 0.3333333333333333703, 0.3333333333333333703, 0.3333333333333333703, 0.3333333333333333703, 0.3333333333333333703, 0.3333333333333333703, 0.3333333333333333703, 0.3333333333333333703, 0.3333333333333333703, 0.3333333333333333703, 0.3333333333333333703, 0.3333333333333333703, 0.3333333333333333703, 0.3333333333333333703, 0.3333333333333333703, 0.3333333333333333703, 0.3333333333333333703, 0.3333333333333333703, 0.3333333333333333703, 0.3333333333333333703, 0.3333333333333333703, 0.3333333333333333703, 0.3333333333333333703, 0.3333333333333333703, 0.3333333333333333703, 0.3333333333333333703, 0.3333333333333333703, 0.3333333333333333703, 0.3333333333333333703, 0.3333333333333333703, 0.3333333333333333703, 0.3333333333333333703, 0.3333333333333333703, 0.3333333333333333703, 0.3333333333333333703, 0.3333333333333333703, 0.3333333333333333703, 0.3333333333333333703, 0.3333333333333333703, 0.3333333333333333703, 0.3333333333333333703, 0.3333333333333333703, 0.3333333333333333703, 0.3333333333333333703, 0.3333333333333333703, 0.3333333333333333703, 0.3333333333333333703, 0.3333333333333333703, 0.3333333333333333703, 0.3333333333333333703, 0.3333333333333333703, 0.3333333333333333703, 0.3333333333333333703, 0.3333333333333333703, 0.3333333333333333703, 0.3333333333333333703, 0.3333333333333333703, 0.3333333333333333703, 0.3333333333333333703, 0.3333333333333333703, 0.3333333333333333703),
 ( 0.3333333333333333703, 0.3333333333333333703, 0.3333333333333333703, 0.3333333333333333703, 0.3333333333333333703, 0.3333333333333333703, 0.3333333333333333703, 0.3333333333333333703, 0.3333333333333333703, 0.3333333333333333703, 0.3333333333333333703, 0.3333333333333333703, 0.3333333333333333703, 0.3333333333333333703, 0.3333333333333333703, 0.3333333333333333703, 0.3333333333333333703, 0.3333333333333333703, 0.3333333333333333703, 0.3333333333333333703, 0.3333333333333333703, 0.3333333333333333703, 0.3333333333333333703, 0.3333333333333333703, 0.3333333333333333703, 0.3333333333333333703, 0.3333333333333333703, 0.3333333333333333703, 0.3333333333333333703, 0.3333333333333333703, 0.3333333333333333703, 0.3333333333333333703, 0.3333333333333333703, 0.3333333333333333703, 0.3333333333333333703, 0.3333333333333333703, 0.3333333333333333703, 0.3333333333333333703, 0.3333333333333333703, 0.3333333333333333703, 0.3333333333333333703, 0.3333333333333333703, 0.3333333333333333703, 0.3333333333333333703, 0.3333333333333333703, 0.3333333333333333703, 0.3333333333333333703, 0.3333333333333333703, 0.3333333333333333703, 0.3333333333333333703, 0.3333333333333333703, 0.3333333333333333703, 0.3333333333333333703, 0.3333333333333333703, 0.3333333333333333703, 0.3333333333333333703, 0.3333333333333333703, 0.3333333333333333703, 0.3333333333333333703, 0.3333333333333333703, 0.3333333333333333703, 0.3333333333333333703, 0.3333333333333333703, 0.3333333333333333703, 0.3333333333333333703, 0.3333333333333333703, 0.3333333333333333703, 0.3333333333333333703, 0.3333333333333333703, 0.3333333333333333703, 0.3333333333333333703, 0.3333333333333333703, 0.3333333333333333703, 0.3333333333333333703, 0.3333333333333333703, 0.3333333333333333703, 0.3333333333333333703, 0.3333333333333333703, 0.3333333333333333703, 0.3333333333333333703, 0.3333333333333333703, 0.3333333333333333703, 0.3333333333333333703, 0.3333333333333333703, 0.3333333333333333703, 0.3333333333333333703, 0.3333333333333333703, 0.3333333333333333703, 0.3333333333333333703, 0.3333333333333333703, 0.3333333333333333703, 0.3333333333333333703, 0.3333333333333333703, 0.3333333333333333703, 0.3333333333333333703, 0.3333333333333333703, 0.3333333333333333703, 0.3333333333333333703, 0.3333333333333333703, 0.3333333333333333703, 0.3333333333333333703, 0.3333333333333333703, 0.3333333333333333703, 0.3333333333333333703, 0.3333333333333333703, 0.3333333333333333703, 0.3333333333333333703, 0.3333333333333333703, 0.3333333333333333703, 0.3333333333333333703, 0.3333333333333333703, 0.3333333333333333703, 0.3333333333333333703, 0.3333333333333333703, 0.3333333333333333703, 0.3333333333333333703, 0.3333333333333333703, 0.3333333333333333703, 0.3333333333333333703, 0.3333333333333333703, 0.3333333333333333703, 0.3333333333333333703, 0.3333333333333333703, 0.3333333333333333703, 0.3333333333333333703, 0.3333333333333333703, 0.3333333333333333703, 0.3333333333333333703, 0.3333333333333333703, 0.3333333333333333703, 0.3333333333333333703, 0.3333333333333333703, 0.3333333333333333703, 0.3333333333333333703, 0.3333333333333333703, 0.3333333333333333703, 0.3333333333333333703, 0.3333333333333333703, 0.3333333333333333703, 0.3333333333333333703, 0.3333333333333333703, 0.3333333333333333703, 0.3333333333333333703, 0.3333333333333333703, 0.3333333333333333703, 0.3333333333333333703, 0.3333333333333333703, 0.3333333333333333703, 0.3333333333333333703, 0.3333333333333333703, 0.3333333333333333703, 0.3333333333333333703, 0.3333333333333333703, 0.3333333333333333703, 0.3333333333333333703, 0.3333333333333333703, 0.3333333333333333703, 0.3333333333333333703, 0.3333333333333333703, 0.3333333333333333703, 0.3333333333333333703, 0.3333333333333333703, 0.3333333333333333703, 0.3333333333333333703, 0.3333333333333333703, 0.3333333333333333703, 0.3333333333333333703, 0.3333333333333333703, 0.3333333333333333703, 0.3333333333333333703, 0.3333333333333333703, 0.3333333333333333703, 0.3333333333333333703, 0.3333333333333333703, 0.3333333333333333703, 0.3333333333333333703, 0.3333333333333333703, 0.3333333333333333703, 0.3333333333333333703, 0.3333333333333333703, 0.3333333333333333703, 0.3333333333333333703, 0.3333333333333333703, 0.3333333333333333703, 0.3333333333333333703, 0.3333333333333333703, 0.3333333333333333703, 0.3333333333333333703, 0.3333333333333333703, 0.3333333333333333703, 0.3333333333333333703, 0.3333333333333333703, 0.3333333333333333703, 0.3333333333333333703, 0.3333333333333333703, 0.3333333333333333703, 0.3333333333333333703, 0.3333333333333333703, 0.3333333333333333703, 0.3333333333333333703, 0.3333333333333333703, 0.3333333333333333703, 0.3333333333333333703, 0.3333333333333333703, 0.3333333333333333703, 0.3333333333333333703, 0.3333333333333333703, 0.3333333333333333703, 0.3333333333333333703, 0.3333333333333333703, 0.3333333333333333703, 0.3333333333333333703, 0.3333333333333333703, 0.3333333333333333703, 0.3333333333333333703, 0.3333333333333333703, 0.3333333333333333703, 0.3333333333333333703, 0.3333333333333333703, 0.3333333333333333703, 0.3333333333333333703, 0.3333333333333333703, 0.3333333333333333703, 0.3333333333333333703, 0.3333333333333333703, 0.3333333333333333703, 0.3333333333333333703, 0.3333333333333333703, 0.3333333333333333703, 0.3333333333333333703, 0.3333333333333333703, 0.3333333333333333703, 0.3333333333333333703, 0.3333333333333333703, 0.3333333333333333703, 0.3333333333333333703, 0.3333333333333333703, 0.3333333333333333703, 0.3333333333333333703, 0.3333333333333333703, 0.3333333333333333703, 0.3333333333333333703, 0.3333333333333333703, 0.3333333333333333703, 0.3333333333333333703, 0.3333333333333333703, 0.3333333333333333703, 0.3333333333333333703, 0.3333333333333333703, 0.3333333333333333703, 0.3333333333333333703, 0.3333333333333333703, 0.3333333333333333703, 0.3333333333333333703, 0.3333333333333333703, 0.3333333333333333703, 0.3333333333333333703, 0.3333333333333333703, 0.3333333333333333703, 0.3333333333333333703, 0.3333333333333333703, 0.3333333333333333703, 0.3333333333333333703, 0.3333333333333333703, 0.3333333333333333703, 0.3333333333333333703, 0.3333333333333333703, 0.3333333333333333703, 0.3333333333333333703, 0.3333333333333333703, 0.3333333333333333703, 0.3333333333333333703, 0.3333333333333333703, 0.3333333333333333703, 0.3333333333333333703, 0.3333333333333333703, 0.3333333333333333703, 0.3333333333333333703, 0.3333333333333333703, 0.3333333333333333703, 0.3333333333333333703, 0.3333333333333333703, 0.3333333333333333703, 0.3333333333333333703, 0.3333333333333333703, 0.3333333333333333703, 0.3333333333333333703, 0.3333333333333333703, 0.3333333333333333703, 0.3333333333333333703, 0.3333333333333333703, 0.3333333333333333703, 0.3333333333333333703, 0.3333333333333333703, 0.3333333333333333703, 0.3333333333333333703, 0.3333333333333333703, 0.3333333333333333703, 0.3333333333333333703, 0.3333333333333333703, 0.3333333333333333703, 0.3333333333333333703, 0.3333333333333333703, 0.3333333333333333703, 0.3333333333333333703, 0.3333333333333333703, 0.3333333333333333703, 0.3333333333333333703, 0.3333333333333333703, 0.3333333333333333703, 0.3333333333333333703, 0.3333333333333333703, 0.3333333333333333703, 0.3333333333333333703, 0.3333333333333333703, 0.3333333333333333703, 0.3333333333333333703, 0.3333333333333333703, 0.3333333333333333703, 0.3333333333333333703, 0.3333333333333333703, 0.3333333333333333703, 0.3333333333333333703, 0.3333333333333333703, 0.3333333333333333703, 0.3333333333333333703, 0.3333333333333333703, 0.3333333333333333703, 0.3333333333333333703, 0.3333333333333333703, 0.3333333333333333703, 0.3333333333333333703, 0.3333333333333333703, 0.3333333333333333703, 0.3333333333333333703, 0.3333333333333333703, 0.3333333333333333703, 0.3333333333333333703, 0.3333333333333333703, 0.3333333333333333703),
 ( 1.000000000000000000, 1.000000000000000000, 1.000000000000000000, 1.000000000000000000, 1.000000000000000000, 1.000000000000000000, 1.000000000000000000, 1.000000000000000000, 1.000000000000000000, 1.000000000000000000, 1.000000000000000000, 1.000000000000000000, 1.000000000000000000, 1.000000000000000000, 1.000000000000000000, 1.000000000000000000, 1.000000000000000000, 1.000000000000000000, 1.000000000000000000, 1.000000000000000000, 1.000000000000000000, 1.000000000000000000, 1.000000000000000000, 1.000000000000000000, 1.000000000000000000, 1.000000000000000000, 1.000000000000000000, 1.000000000000000000, 1.000000000000000000, 1.000000000000000000, 1.000000000000000000, 1.000000000000000000, 1.000000000000000000, 1.000000000000000000, 1.000000000000000000, 1.000000000000000000, 1.000000000000000000, 1.000000000000000000, 1.000000000000000000, 1.000000000000000000, 1.000000000000000000, 1.000000000000000000, 1.000000000000000000, 1.000000000000000000, 1.000000000000000000, 1.000000000000000000, 1.000000000000000000, 1.000000000000000000, 1.000000000000000000, 1.000000000000000000, 1.000000000000000000, 1.000000000000000000, 1.000000000000000000, 1.000000000000000000, 1.000000000000000000, 1.000000000000000000, 1.000000000000000000, 1.000000000000000000, 1.000000000000000000, 1.000000000000000000, 1.000000000000000000, 1.000000000000000000, 1.000000000000000000, 1.000000000000000000, 1.000000000000000000, 1.000000000000000000, 1.000000000000000000, 1.000000000000000000, 1.000000000000000000, 1.000000000000000000, 1.000000000000000000, 1.000000000000000000, 1.000000000000000000, 1.000000000000000000, 1.000000000000000000, 1.000000000000000000, 1.000000000000000000, 1.000000000000000000, 1.000000000000000000, 1.000000000000000000, 1.000000000000000000, 1.000000000000000000, 1.000000000000000000, 1.000000000000000000, 1.000000000000000000, 1.000000000000000000, 1.000000000000000000, 1.000000000000000000, 1.000000000000000000, 1.000000000000000000, 1.000000000000000000, 1.000000000000000000, 1.000000000000000000, 1.000000000000000000, 1.000000000000000000, 1.000000000000000000, 1.000000000000000000, 1.000000000000000000, 1.000000000000000000, 1.000000000000000000, 1.000000000000000000, 1.000000000000000000, 1.000000000000000000, 1.000000000000000000, 1.000000000000000000, 1.000000000000000000, 1.000000000000000000, 1.000000000000000000, 1.000000000000000000, 1.000000000000000000, 1.000000000000000000, 1.000000000000000000, 1.000000000000000000, 1.000000000000000000, 1.000000000000000000, 1.000000000000000000, 1.000000000000000000, 1.000000000000000000, 1.000000000000000000, 1.000000000000000000, 1.000000000000000000, 1.000000000000000000, 1.000000000000000000, 1.000000000000000000, 1.000000000000000000, 1.000000000000000000, 1.000000000000000000, 1.000000000000000000, 1.000000000000000000, 1.000000000000000000, 1.000000000000000000, 1.000000000000000000, 1.000000000000000000, 1.000000000000000000, 1.000000000000000000, 1.000000000000000000, 1.000000000000000000, 1.000000000000000000, 1.000000000000000000, 1.000000000000000000, 1.000000000000000000, 1.000000000000000000, 1.000000000000000000, 1.000000000000000000, 1.000000000000000000, 1.000000000000000000, 1.000000000000000000, 1.000000000000000000, 1.000000000000000000, 1.000000000000000000, 1.000000000000000000, 1.000000000000000000, 1.000000000000000000, 1.000000000000000000, 1.000000000000000000, 1.000000000000000000, 1.000000000000000000, 1.000000000000000000, 1.000000000000000000, 1.000000000000000000, 1.000000000000000000, 1.000000000000000000, 1.000000000000000000, 1.000000000000000000, 1.000000000000000000, 1.000000000000000000, 1.000000000000000000, 1.000000000000000000, 1.000000000000000000, 1.000000000000000000, 1.000000000000000000, 1.000000000000000000, 1.000000000000000000, 1.000000000000000000, 1.000000000000000000, 1.000000000000000000, 1.000000000000000000, 1.000000000000000000, 1.000000000000000000, 1.000000000000000000, 1.000000000000000000, 1.000000000000000000, 1.000000000000000000, 1.000000000000000000, 1.000000000000000000, 1.000000000000000000, 1.000000000000000000, 1.000000000000000000, 1.000000000000000000, 1.000000000000000000, 1.000000000000000000, 1.000000000000000000, 1.000000000000000000, 1.000000000000000000, 1.000000000000000000, 1.000000000000000000, 1.000000000000000000, 1.000000000000000000, 1.000000000000000000, 1.000000000000000000, 1.000000000000000000, 1.000000000000000000, 1.000000000000000000, 1.000000000000000000, 1.000000000000000000, 1.000000000000000000, 1.000000000000000000, 1.000000000000000000, 1.000000000000000000, 1.000000000000000000, 1.000000000000000000, 1.000000000000000000, 1.000000000000000000, 1.000000000000000000, 1.000000000000000000, 1.000000000000000000, 1.000000000000000000, 1.000000000000000000, 1.000000000000000000, 1.000000000000000000, 1.000000000000000000, 1.000000000000000000, 1.000000000000000000, 1.000000000000000000, 1.000000000000000000, 1.000000000000000000, 1.000000000000000000, 1.000000000000000000, 1.000000000000000000, 1.000000000000000000, 1.000000000000000000, 1.000000000000000000, 1.000000000000000000, 1.000000000000000000, 1.000000000000000000, 1.000000000000000000, 1.000000000000000000, 1.000000000000000000, 1.000000000000000000, 1.000000000000000000, 1.000000000000000000, 1.000000000000000000, 1.000000000000000000, 1.000000000000000000, 1.000000000000000000, 1.000000000000000000, 1.000000000000000000, 1.000000000000000000, 1.000000000000000000, 1.000000000000000000, 1.000000000000000000, 1.000000000000000000, 1.000000000000000000, 1.000000000000000000, 1.000000000000000000, 1.000000000000000000, 1.000000000000000000, 1.000000000000000000, 1.000000000000000000, 1.000000000000000000, 1.000000000000000000, 1.000000000000000000, 1.000000000000000000, 1.000000000000000000, 1.000000000000000000, 1.000000000000000000, 1.000000000000000000, 1.000000000000000000, 1.000000000000000000, 1.000000000000000000, 1.000000000000000000, 1.000000000000000000, 1.000000000000000000, 1.000000000000000000, 1.000000000000000000, 1.000000000000000000, 1.000000000000000000, 1.000000000000000000, 1.000000000000000000, 1.000000000000000000, 1.000000000000000000, 1.000000000000000000, 1.000000000000000000, 1.000000000000000000, 1.000000000000000000, 1.000000000000000000, 1.000000000000000000, 1.000000000000000000, 1.000000000000000000, 1.000000000000000000, 1.000000000000000000, 1.000000000000000000, 1.000000000000000000, 1.000000000000000000, 1.000000000000000000, 1.000000000000000000, 1.000000000000000000, 1.000000000000000000, 1.000000000000000000, 1.000000000000000000, 1.000000000000000000, 1.000000000000000000, 1.000000000000000000, 1.000000000000000000, 1.000000000000000000, 1.000000000000000000, 1.000000000000000000, 1.000000000000000000, 1.000000000000000000, 1.000000000000000000, 1.000000000000000000, 1.000000000000000000, 1.000000000000000000, 1.000000000000000000, 1.000000000000000000, 1.000000000000000000, 1.000000000000000000, 1.000000000000000000, 1.000000000000000000, 1.000000000000000000, 1.000000000000000000, 1.000000000000000000, 1.000000000000000000, 1.000000000000000000, 1.000000000000000000, 1.000000000000000000, 1.000000000000000000, 1.000000000000000000, 1.000000000000000000, 1.000000000000000000, 1.000000000000000000, 1.000000000000000000, 1.000000000000000000, 1.000000000000000000, 1.000000000000000000, 1.000000000000000000, 1.000000000000000000, 1.000000000000000000, 1.000000000000000000, 1.000000000000000000),
 ( 0.3333333333333333703, 0.3333333333333333703, 0.3333333333333333703, 0.3333333333333333703, 0.3333333333333333703, 0.3333333333333333703, 0.3333333333333333703, 0.3333333333333333703, 0.3333333333333333703, 0.3333333333333333703, 0.3333333333333333703, 0.3333333333333333703, 0.3333333333333333703, 0.3333333333333333703, 0.3333333333333333703, 0.3333333333333333703, 0.3333333333333333703, 0.3333333333333333703, 0.3333333333333333703, 0.3333333333333333703, 0.3333333333333333703, 0.3333333333333333703, 0.3333333333333333703, 0.3333333333333333703, 0.3333333333333333703, 0.3333333333333333703, 0.3333333333333333703, 0.3333333333333333703, 0.3333333333333333703, 0.3333333333333333703, 0.3333333333333333703, 0.3333333333333333703, 0.3333333333333333703, 0.3333333333333333703, 0.3333333333333333703, 0.3333333333333333703, 0.3333333333333333703, 0.3333333333333333703, 0.3333333333333333703, 0.3333333333333333703, 0.3333333333333333703, 0.3333333333333333703, 0.3333333333333333703, 0.3333333333333333703, 0.3333333333333333703, 0.3333333333333333703, 0.3333333333333333703, 0.3333333333333333703, 0.3333333333333333703, 0.3333333333333333703, 0.3333333333333333703, 0.3333333333333333703, 0.3333333333333333703, 0.3333333333333333703, 0.3333333333333333703, 0.3333333333333333703, 0.3333333333333333703, 0.3333333333333333703, 0.3333333333333333703, 0.3333333333333333703, 0.3333333333333333703, 0.3333333333333333703, 0.3333333333333333703, 0.3333333333333333703, 0.3333333333333333703, 0.3333333333333333703, 0.3333333333333333703, 0.3333333333333333703, 0.3333333333333333703, 0.3333333333333333703, 0.3333333333333333703, 0.3333333333333333703, 0.3333333333333333703, 0.3333333333333333703, 0.3333333333333333703, 0.3333333333333333703, 0.3333333333333333703, 0.3333333333333333703, 0.3333333333333333703, 0.3333333333333333703, 0.3333333333333333703, 0.3333333333333333703, 0.3333333333333333703, 0.3333333333333333703, 0.3333333333333333703, 0.3333333333333333703, 0.3333333333333333703, 0.3333333333333333703, 0.3333333333333333703, 0.3333333333333333703, 0.3333333333333333703, 0.3333333333333333703, 0.3333333333333333703, 0.3333333333333333703, 0.3333333333333333703, 0.3333333333333333703, 0.3333333333333333703, 0.3333333333333333703, 0.3333333333333333703, 0.3333333333333333703, 0.3333333333333333703, 0.3333333333333333703, 0.3333333333333333703, 0.3333333333333333703, 0.3333333333333333703, 0.3333333333333333703, 0.3333333333333333703, 0.3333333333333333703, 0.3333333333333333703, 0.3333333333333333703, 0.3333333333333333703, 0.3333333333333333703, 0.3333333333333333703, 0.3333333333333333703, 0.3333333333333333703, 0.3333333333333333703, 0.3333333333333333703, 0.3333333333333333703, 0.3333333333333333703, 0.3333333333333333703, 0.3333333333333333703, 0.3333333333333333703, 0.3333333333333333703, 0.3333333333333333703, 0.3333333333333333703, 0.3333333333333333703, 0.3333333333333333703, 0.3333333333333333703, 0.3333333333333333703, 0.3333333333333333703, 0.3333333333333333703, 0.3333333333333333703, 0.3333333333333333703, 0.3333333333333333703, 0.3333333333333333703, 0.3333333333333333703, 0.3333333333333333703, 0.3333333333333333703, 0.3333333333333333703, 0.3333333333333333703, 0.3333333333333333703, 0.3333333333333333703, 0.3333333333333333703, 0.3333333333333333703, 0.3333333333333333703, 0.3333333333333333703, 0.3333333333333333703, 0.3333333333333333703, 0.3333333333333333703, 0.3333333333333333703, 0.3333333333333333703, 0.3333333333333333703, 0.3333333333333333703, 0.3333333333333333703, 0.3333333333333333703, 0.3333333333333333703, 0.3333333333333333703, 0.3333333333333333703, 0.3333333333333333703, 0.3333333333333333703, 0.3333333333333333703, 0.3333333333333333703, 0.3333333333333333703, 0.3333333333333333703, 0.3333333333333333703, 0.3333333333333333703, 0.3333333333333333703, 0.3333333333333333703, 0.3333333333333333703, 0.3333333333333333703, 0.3333333333333333703, 0.3333333333333333703, 0.3333333333333333703, 0.3333333333333333703, 0.3333333333333333703, 0.3333333333333333703, 0.3333333333333333703, 0.3333333333333333703, 0.3333333333333333703, 0.3333333333333333703, 0.3333333333333333703, 0.3333333333333333703, 0.3333333333333333703, 0.3333333333333333703, 0.3333333333333333703, 0.3333333333333333703, 0.3333333333333333703, 0.3333333333333333703, 0.3333333333333333703, 0.3333333333333333703, 0.3333333333333333703, 0.3333333333333333703, 0.3333333333333333703, 0.3333333333333333703, 0.3333333333333333703, 0.3333333333333333703, 0.3333333333333333703, 0.3333333333333333703, 0.3333333333333333703, 0.3333333333333333703, 0.3333333333333333703, 0.3333333333333333703, 0.3333333333333333703, 0.3333333333333333703, 0.3333333333333333703, 0.3333333333333333703, 0.3333333333333333703, 0.3333333333333333703, 0.3333333333333333703, 0.3333333333333333703, 0.3333333333333333703, 0.3333333333333333703, 0.3333333333333333703, 0.3333333333333333703, 0.3333333333333333703, 0.3333333333333333703, 0.3333333333333333703, 0.3333333333333333703, 0.3333333333333333703, 0.3333333333333333703, 0.3333333333333333703, 0.3333333333333333703, 0.3333333333333333703, 0.3333333333333333703, 0.3333333333333333703, 0.3333333333333333703, 0.3333333333333333703, 0.3333333333333333703, 0.3333333333333333703, 0.3333333333333333703, 0.3333333333333333703, 0.3333333333333333703, 0.3333333333333333703, 0.3333333333333333703, 0.3333333333333333703, 0.3333333333333333703, 0.3333333333333333703, 0.3333333333333333703, 0.3333333333333333703, 0.3333333333333333703, 0.3333333333333333703, 0.3333333333333333703, 0.3333333333333333703, 0.3333333333333333703, 0.3333333333333333703, 0.3333333333333333703, 0.3333333333333333703, 0.3333333333333333703, 0.3333333333333333703, 0.3333333333333333703, 0.3333333333333333703, 0.3333333333333333703, 0.3333333333333333703, 0.3333333333333333703, 0.3333333333333333703, 0.3333333333333333703, 0.3333333333333333703, 0.3333333333333333703, 0.3333333333333333703, 0.3333333333333333703, 0.3333333333333333703, 0.3333333333333333703, 0.3333333333333333703, 0.3333333333333333703, 0.3333333333333333703, 0.3333333333333333703, 0.3333333333333333703, 0.3333333333333333703, 0.3333333333333333703, 0.3333333333333333703, 0.3333333333333333703, 0.3333333333333333703, 0.3333333333333333703, 0.3333333333333333703, 0.3333333333333333703, 0.3333333333333333703, 0.3333333333333333703, 0.3333333333333333703, 0.3333333333333333703, 0.3333333333333333703, 0.3333333333333333703, 0.3333333333333333703, 0.3333333333333333703, 0.3333333333333333703, 0.3333333333333333703, 0.3333333333333333703, 0.3333333333333333703, 0.3333333333333333703, 0.3333333333333333703, 0.3333333333333333703, 0.3333333333333333703, 0.3333333333333333703, 0.3333333333333333703, 0.3333333333333333703, 0.3333333333333333703, 0.3333333333333333703, 0.3333333333333333703, 0.3333333333333333703, 0.3333333333333333703, 0.3333333333333333703, 0.3333333333333333703, 0.3333333333333333703, 0.3333333333333333703, 0.3333333333333333703, 0.3333333333333333703, 0.3333333333333333703, 0.3333333333333333703, 0.3333333333333333703, 0.3333333333333333703, 0.3333333333333333703, 0.3333333333333333703, 0.3333333333333333703, 0.3333333333333333703, 0.3333333333333333703, 0.3333333333333333703, 0.3333333333333333703, 0.3333333333333333703, 0.3333333333333333703, 0.3333333333333333703, 0.3333333333333333703, 0.3333333333333333703, 0.3333333333333333703, 0.3333333333333333703, 0.3333333333333333703, 0.3333333333333333703, 0.3333333333333333703, 0.3333333333333333703, 0.3333333333333333703, 0.3333333333333333703, 0.3333333333333333703, 0.3333333333333333703, 0.3333333333333333703, 0.3333333333333333703, 0.3333333333333333703, 0.3333333333333333703, 0.3333333333333333703, 0.3333333333333333703, 0.3333333333333333703, 0.3333333333333333703, 0.3333333333333333703),
 ( 0.3333333333333333703, 0.3333333333333333703, 0.3333333333333333703, 0.3333333333333333703, 0.3333333333333333703, 0.3333333333333333703, 0.3333333333333333703, 0.3333333333333333703, 0.3333333333333333703, 0.3333333333333333703, 0.3333333333333333703, 0.3333333333333333703, 0.3333333333333333703, 0.3333333333333333703, 0.3333333333333333703, 0.3333333333333333703, 0.3333333333333333703, 0.3333333333333333703, 0.3333333333333333703, 0.3333333333333333703, 0.3333333333333333703, 0.3333333333333333703, 0.3333333333333333703, 0.3333333333333333703, 0.3333333333333333703, 0.3333333333333333703, 0.3333333333333333703, 0.3333333333333333703, 0.3333333333333333703, 0.3333333333333333703, 0.3333333333333333703, 0.3333333333333333703, 0.3333333333333333703, 0.3333333333333333703, 0.3333333333333333703, 0.3333333333333333703, 0.3333333333333333703, 0.3333333333333333703, 0.3333333333333333703, 0.3333333333333333703, 0.3333333333333333703, 0.3333333333333333703, 0.3333333333333333703, 0.3333333333333333703, 0.3333333333333333703, 0.3333333333333333703, 0.3333333333333333703, 0.3333333333333333703, 0.3333333333333333703, 0.3333333333333333703, 0.3333333333333333703, 0.3333333333333333703, 0.3333333333333333703, 0.3333333333333333703, 0.3333333333333333703, 0.3333333333333333703, 0.3333333333333333703, 0.3333333333333333703, 0.3333333333333333703, 0.3333333333333333703, 0.3333333333333333703, 0.3333333333333333703, 0.3333333333333333703, 0.3333333333333333703, 0.3333333333333333703, 0.3333333333333333703, 0.3333333333333333703, 0.3333333333333333703, 0.3333333333333333703, 0.3333333333333333703, 0.3333333333333333703, 0.3333333333333333703, 0.3333333333333333703, 0.3333333333333333703, 0.3333333333333333703, 0.3333333333333333703, 0.3333333333333333703, 0.3333333333333333703, 0.3333333333333333703, 0.3333333333333333703, 0.3333333333333333703, 0.3333333333333333703, 0.3333333333333333703, 0.3333333333333333703, 0.3333333333333333703, 0.3333333333333333703, 0.3333333333333333703, 0.3333333333333333703, 0.3333333333333333703, 0.3333333333333333703, 0.3333333333333333703, 0.3333333333333333703, 0.3333333333333333703, 0.3333333333333333703, 0.3333333333333333703, 0.3333333333333333703, 0.3333333333333333703, 0.3333333333333333703, 0.3333333333333333703, 0.3333333333333333703, 0.3333333333333333703, 0.3333333333333333703, 0.3333333333333333703, 0.3333333333333333703, 0.3333333333333333703, 0.3333333333333333703, 0.3333333333333333703, 0.3333333333333333703, 0.3333333333333333703, 0.3333333333333333703, 0.3333333333333333703, 0.3333333333333333703, 0.3333333333333333703, 0.3333333333333333703, 0.3333333333333333703, 0.3333333333333333703, 0.3333333333333333703, 0.3333333333333333703, 0.3333333333333333703, 0.3333333333333333703, 0.3333333333333333703, 0.3333333333333333703, 0.3333333333333333703, 0.3333333333333333703, 0.3333333333333333703, 0.3333333333333333703, 0.3333333333333333703, 0.3333333333333333703, 0.3333333333333333703, 0.3333333333333333703, 0.3333333333333333703, 0.3333333333333333703, 0.3333333333333333703, 0.3333333333333333703, 0.3333333333333333703, 0.3333333333333333703, 0.3333333333333333703, 0.3333333333333333703, 0.3333333333333333703, 0.3333333333333333703, 0.3333333333333333703, 0.3333333333333333703, 0.3333333333333333703, 0.3333333333333333703, 0.3333333333333333703, 0.3333333333333333703, 0.3333333333333333703, 0.3333333333333333703, 0.3333333333333333703, 0.3333333333333333703, 0.3333333333333333703, 0.3333333333333333703, 0.3333333333333333703, 0.3333333333333333703, 0.3333333333333333703, 0.3333333333333333703, 0.3333333333333333703, 0.3333333333333333703, 0.3333333333333333703, 0.3333333333333333703, 0.3333333333333333703, 0.3333333333333333703, 0.3333333333333333703, 0.3333333333333333703, 0.3333333333333333703, 0.3333333333333333703, 0.3333333333333333703, 0.3333333333333333703, 0.3333333333333333703, 0.3333333333333333703, 0.3333333333333333703, 0.3333333333333333703, 0.3333333333333333703, 0.3333333333333333703, 0.3333333333333333703, 0.3333333333333333703, 0.3333333333333333703, 0.3333333333333333703, 0.3333333333333333703, 0.3333333333333333703, 0.3333333333333333703, 0.3333333333333333703, 0.3333333333333333703, 0.3333333333333333703, 0.3333333333333333703, 0.3333333333333333703, 0.3333333333333333703, 0.3333333333333333703, 0.3333333333333333703, 0.3333333333333333703, 0.3333333333333333703, 0.3333333333333333703, 0.3333333333333333703, 0.3333333333333333703, 0.3333333333333333703, 0.3333333333333333703, 0.3333333333333333703, 0.3333333333333333703, 0.3333333333333333703, 0.3333333333333333703, 0.3333333333333333703, 0.3333333333333333703, 0.3333333333333333703, 0.3333333333333333703, 0.3333333333333333703, 0.3333333333333333703, 0.3333333333333333703, 0.3333333333333333703, 0.3333333333333333703, 0.3333333333333333703, 0.3333333333333333703, 0.3333333333333333703, 0.3333333333333333703, 0.3333333333333333703, 0.3333333333333333703, 0.3333333333333333703, 0.3333333333333333703, 0.3333333333333333703, 0.3333333333333333703, 0.3333333333333333703, 0.3333333333333333703, 0.3333333333333333703, 0.3333333333333333703, 0.3333333333333333703, 0.3333333333333333703, 0.3333333333333333703, 0.3333333333333333703, 0.3333333333333333703, 0.3333333333333333703, 0.3333333333333333703, 0.3333333333333333703, 0.3333333333333333703, 0.3333333333333333703, 0.3333333333333333703, 0.3333333333333333703, 0.3333333333333333703, 0.3333333333333333703, 0.3333333333333333703, 0.3333333333333333703, 0.3333333333333333703, 0.3333333333333333703, 0.3333333333333333703, 0.3333333333333333703, 0.3333333333333333703, 0.3333333333333333703, 0.3333333333333333703, 0.3333333333333333703, 0.3333333333333333703, 0.3333333333333333703, 0.3333333333333333703, 0.3333333333333333703, 0.3333333333333333703, 0.3333333333333333703, 0.3333333333333333703, 0.3333333333333333703, 0.3333333333333333703, 0.3333333333333333703, 0.3333333333333333703, 0.3333333333333333703, 0.3333333333333333703, 0.3333333333333333703, 0.3333333333333333703, 0.3333333333333333703, 0.3333333333333333703, 0.3333333333333333703, 0.3333333333333333703, 0.3333333333333333703, 0.3333333333333333703, 0.3333333333333333703, 0.3333333333333333703, 0.3333333333333333703, 0.3333333333333333703, 0.3333333333333333703, 0.3333333333333333703, 0.3333333333333333703, 0.3333333333333333703, 0.3333333333333333703, 0.3333333333333333703, 0.3333333333333333703, 0.3333333333333333703, 0.3333333333333333703, 0.3333333333333333703, 0.3333333333333333703, 0.3333333333333333703, 0.3333333333333333703, 0.3333333333333333703, 0.3333333333333333703, 0.3333333333333333703, 0.3333333333333333703, 0.3333333333333333703, 0.3333333333333333703, 0.3333333333333333703, 0.3333333333333333703, 0.3333333333333333703, 0.3333333333333333703, 0.3333333333333333703, 0.3333333333333333703, 0.3333333333333333703, 0.3333333333333333703, 0.3333333333333333703, 0.3333333333333333703, 0.3333333333333333703, 0.3333333333333333703, 0.3333333333333333703, 0.3333333333333333703, 0.3333333333333333703, 0.3333333333333333703, 0.3333333333333333703, 0.3333333333333333703, 0.3333333333333333703, 0.3333333333333333703, 0.3333333333333333703, 0.3333333333333333703, 0.3333333333333333703, 0.3333333333333333703, 0.3333333333333333703, 0.3333333333333333703, 0.3333333333333333703, 0.3333333333333333703, 0.3333333333333333703, 0.3333333333333333703, 0.3333333333333333703, 0.3333333333333333703, 0.3333333333333333703, 0.3333333333333333703, 0.3333333333333333703, 0.3333333333333333703, 0.3333333333333333703, 0.3333333333333333703, 0.3333333333333333703, 0.3333333333333333703, 0.3333333333333333703, 0.3333333333333333703, 0.3333333333333333703, 0.3333333333333333703, 0.3333333333333333703, 0.3333333333333333703, 0.3333333333333333703, 0.3333333333333333703, 0.3333333333333333703),
 ( 1.000000000000000000, 1.000000000000000000, 1.000000000000000000, 1.000000000000000000, 1.000000000000000000, 1.000000000000000000, 1.000000000000000000, 1.000000000000000000, 1.000000000000000000, 1.000000000000000000, 1.000000000000000000, 1.000000000000000000, 1.000000000000000000, 1.000000000000000000, 1.000000000000000000, 1.000000000000000000, 1.000000000000000000, 1.000000000000000000, 1.000000000000000000, 1.000000000000000000, 1.000000000000000000, 1.000000000000000000, 1.000000000000000000, 1.000000000000000000, 1.000000000000000000, 1.000000000000000000, 1.000000000000000000, 1.000000000000000000, 1.000000000000000000, 1.000000000000000000, 1.000000000000000000, 1.000000000000000000, 1.000000000000000000, 1.000000000000000000, 1.000000000000000000, 1.000000000000000000, 1.000000000000000000, 1.000000000000000000, 1.000000000000000000, 1.000000000000000000, 1.000000000000000000, 1.000000000000000000, 1.000000000000000000, 1.000000000000000000, 1.000000000000000000, 1.000000000000000000, 1.000000000000000000, 1.000000000000000000, 1.000000000000000000, 1.000000000000000000, 1.000000000000000000, 1.000000000000000000, 1.000000000000000000, 1.000000000000000000, 1.000000000000000000, 1.000000000000000000, 1.000000000000000000, 1.000000000000000000, 1.000000000000000000, 1.000000000000000000, 1.000000000000000000, 1.000000000000000000, 1.000000000000000000, 1.000000000000000000, 1.000000000000000000, 1.000000000000000000, 1.000000000000000000, 1.000000000000000000, 1.000000000000000000, 1.000000000000000000, 1.000000000000000000, 1.000000000000000000, 1.000000000000000000, 1.000000000000000000, 1.000000000000000000, 1.000000000000000000, 1.000000000000000000, 1.000000000000000000, 1.000000000000000000, 1.000000000000000000, 1.000000000000000000, 1.000000000000000000, 1.000000000000000000, 1.000000000000000000, 1.000000000000000000, 1.000000000000000000, 1.000000000000000000, 1.000000000000000000, 1.000000000000000000, 1.000000000000000000, 1.000000000000000000, 1.000000000000000000, 1.000000000000000000, 1.000000000000000000, 1.000000000000000000, 1.000000000000000000, 1.000000000000000000, 1.000000000000000000, 1.000000000000000000, 1.000000000000000000, 1.000000000000000000, 1.000000000000000000, 1.000000000000000000, 1.000000000000000000, 1.000000000000000000, 1.000000000000000000, 1.000000000000000000, 1.000000000000000000, 1.000000000000000000, 1.000000000000000000, 1.000000000000000000, 1.000000000000000000, 1.000000000000000000, 1.000000000000000000, 1.000000000000000000, 1.000000000000000000, 1.000000000000000000, 1.000000000000000000, 1.000000000000000000, 1.000000000000000000, 1.000000000000000000, 1.000000000000000000, 1.000000000000000000, 1.000000000000000000, 1.000000000000000000, 1.000000000000000000, 1.000000000000000000, 1.000000000000000000, 1.000000000000000000, 1.000000000000000000, 1.000000000000000000, 1.000000000000000000, 1.000000000000000000, 1.000000000000000000, 1.000000000000000000, 1.000000000000000000, 1.000000000000000000, 1.000000000000000000, 1.000000000000000000, 1.000000000000000000, 1.000000000000000000, 1.000000000000000000, 1.000000000000000000, 1.000000000000000000, 1.000000000000000000, 1.000000000000000000, 1.000000000000000000, 1.000000000000000000, 1.000000000000000000, 1.000000000000000000, 1.000000000000000000, 1.000000000000000000, 1.000000000000000000, 1.000000000000000000, 1.000000000000000000, 1.000000000000000000, 1.000000000000000000, 1.000000000000000000, 1.000000000000000000, 1.000000000000000000, 1.000000000000000000, 1.000000000000000000, 1.000000000000000000, 1.000000000000000000, 1.000000000000000000, 1.000000000000000000, 1.000000000000000000, 1.000000000000000000, 1.000000000000000000, 1.000000000000000000, 1.000000000000000000, 1.000000000000000000, 1.000000000000000000, 1.000000000000000000, 1.000000000000000000, 1.000000000000000000, 1.000000000000000000, 1.000000000000000000, 1.000000000000000000, 1.000000000000000000, 1.000000000000000000, 1.000000000000000000, 1.000000000000000000, 1.000000000000000000, 1.000000000000000000, 1.000000000000000000, 1.000000000000000000, 1.000000000000000000, 1.000000000000000000, 1.000000000000000000, 1.000000000000000000, 1.000000000000000000, 1.000000000000000000, 1.000000000000000000, 1.000000000000000000, 1.000000000000000000, 1.000000000000000000, 1.000000000000000000, 1.000000000000000000, 1.000000000000000000, 1.000000000000000000, 1.000000000000000000, 1.000000000000000000, 1.000000000000000000, 1.000000000000000000, 1.000000000000000000, 1.000000000000000000, 1.000000000000000000, 1.000000000000000000, 1.000000000000000000, 1.000000000000000000, 1.000000000000000000, 1.000000000000000000, 1.000000000000000000, 1.000000000000000000, 1.000000000000000000, 1.000000000000000000, 1.000000000000000000, 1.000000000000000000, 1.000000000000000000, 1.000000000000000000, 1.000000000000000000, 1.000000000000000000, 1.000000000000000000, 1.000000000000000000, 1.000000000000000000, 1.000000000000000000, 1.000000000000000000, 1.000000000000000000, 1.000000000000000000, 1.000000000000000000, 1.000000000000000000, 1.000000000000000000, 1.000000000000000000, 1.000000000000000000, 1.000000000000000000, 1.000000000000000000, 1.000000000000000000, 1.000000000000000000, 1.000000000000000000, 1.000000000000000000, 1.000000000000000000, 1.000000000000000000, 1.000000000000000000, 1.000000000000000000, 1.000000000000000000, 1.000000000000000000, 1.000000000000000000, 1.000000000000000000, 1.000000000000000000, 1.000000000000000000, 1.000000000000000000, 1.000000000000000000, 1.000000000000000000, 1.000000000000000000, 1.000000000000000000, 1.000000000000000000, 1.000000000000000000, 1.000000000000000000, 1.000000000000000000, 1.000000000000000000, 1.000000000000000000, 1.000000000000000000, 1.000000000000000000, 1.000000000000000000, 1.000000000000000000, 1.000000000000000000, 1.000000000000000000, 1.000000000000000000, 1.000000000000000000, 1.000000000000000000, 1.000000000000000000, 1.000000000000000000, 1.000000000000000000, 1.000000000000000000, 1.000000000000000000, 1.000000000000000000, 1.000000000000000000, 1.000000000000000000, 1.000000000000000000, 1.000000000000000000, 1.000000000000000000, 1.000000000000000000, 1.000000000000000000, 1.000000000000000000, 1.000000000000000000, 1.000000000000000000, 1.000000000000000000, 1.000000000000000000, 1.000000000000000000, 1.000000000000000000, 1.000000000000000000, 1.000000000000000000, 1.000000000000000000, 1.000000000000000000, 1.000000000000000000, 1.000000000000000000, 1.000000000000000000, 1.000000000000000000, 1.000000000000000000, 1.000000000000000000, 1.000000000000000000, 1.000000000000000000, 1.000000000000000000, 1.000000000000000000, 1.000000000000000000, 1.000000000000000000, 1.000000000000000000, 1.000000000000000000, 1.000000000000000000, 1.000000000000000000, 1.000000000000000000, 1.000000000000000000, 1.000000000000000000, 1.000000000000000000, 1.000000000000000000, 1.000000000000000000, 1.000000000000000000, 1.000000000000000000, 1.000000000000000000, 1.000000000000000000, 1.000000000000000000, 1.000000000000000000, 1.000000000000000000, 1.000000000000000000, 1.000000000000000000, 1.000000000000000000, 1.000000000000000000, 1.000000000000000000, 1.000000000000000000, 1.000000000000000000, 1.000000000000000000, 1.000000000000000000, 1.000000000000000000, 1.000000000000000000, 1.000000000000000000, 1.000000000000000000, 1.000000000000000000, 1.000000000000000000, 1.000000000000000000) ) ) 
 REPRESENTATION_ITEM ( '' )  SURFACE ( )  );
#6873 = FILL_AREA_STYLE_COLOUR ( '', #15337 ) ;
#6874 = CARTESIAN_POINT ( 'NONE',  ( 5.920964624126254350, -19.79845160325395526, -232.2234910544682123 ) ) ;
#6875 = CARTESIAN_POINT ( 'NONE',  ( -27.52457542293397097, 5.447957517019466067, -230.2717933641555135 ) ) ;
#6876 = CARTESIAN_POINT ( 'NONE',  ( 10.31623634631035991, 26.83927646318382898, -220.2315638557092541 ) ) ;
#6877 = CARTESIAN_POINT ( 'NONE',  ( -9.491065840222427497, 13.31995980477872266, -232.8537120564120073 ) ) ;
#6878 = ORIENTED_EDGE ( 'NONE', *, *, #14385, .F. ) ;
#6879 = CARTESIAN_POINT ( 'NONE',  ( 24.04182214053767908, -5.779968796880146975, -234.9365023861272164 ) ) ;
#6880 = EDGE_LOOP ( 'NONE', ( #22032, #6100, #5370, #893 ) ) ;
#6881 = CARTESIAN_POINT ( 'NONE',  ( 22.84140515590350518, 18.29101041979067332, -226.2334522600520472 ) ) ;
#6882 = EDGE_CURVE ( 'NONE', #1930, #2334, #15679, .T. ) ;
#6883 = CARTESIAN_POINT ( 'NONE',  ( -11.94727018630768178, 9.025563988971828877, -220.6148682757971358 ) ) ;
#6884 = CARTESIAN_POINT ( 'NONE',  ( -13.63002737749749826, 6.315035547785179837, -227.0490028799284516 ) ) ;
#6885 = CARTESIAN_POINT ( 'NONE',  ( -12.79488508867961549, -11.10380203712096581, -230.9440799972209106 ) ) ;
#6886 = CARTESIAN_POINT ( 'NONE',  ( 2.999999999999970690, 6.000000000000006217, -221.9999999999999716 ) ) ;
#6887 = CARTESIAN_POINT ( 'NONE',  ( 29.89309326230132058, 6.052383583152112223, -228.3539431708548477 ) ) ;
#6888 = CARTESIAN_POINT ( 'NONE',  ( -24.92290506463145405, 6.124412323591598373, -220.3779252408000104 ) ) ;
#6889 = CARTESIAN_POINT ( 'NONE',  ( 13.85207896949186335, 7.847214149978243292, -217.3457543576531066 ) ) ;
#6890 = CARTESIAN_POINT ( 'NONE',  ( 21.18605525173251891, 3.426801613781890854, -232.1183243183448894 ) ) ;
#6891 = CARTESIAN_POINT ( 'NONE',  ( -9.935407011182972425, -19.19496561732008999, -215.7587022423821850 ) ) ;
#6892 = CIRCLE ( 'NONE', #12288, 25.00000000000000000 ) ;
#6893 = ORIENTED_EDGE ( 'NONE', *, *, #5207, .T. ) ;
#6894 = CARTESIAN_POINT ( 'NONE',  ( -9.776740361816679936, -16.43846667899986258, -218.0739489017842061 ) ) ;
#6895 = CARTESIAN_POINT ( 'NONE',  ( -5.607934827417612844, 15.68271927908880770, -232.1026723719274969 ) ) ;
#6896 = CARTESIAN_POINT ( 'NONE',  ( 14.99336262864975211, -23.54026314425397004, -231.3018640253376361 ) ) ;
#6897 = CARTESIAN_POINT ( 'NONE',  ( -9.517741096562200909, 20.63709896626785678, -234.1036702156204967 ) ) ;
#6898 = CARTESIAN_POINT ( 'NONE',  ( 10.25809576580632232, -7.052396458808492419, -221.5466685117269208 ) ) ;
#6899 = CARTESIAN_POINT ( 'NONE',  ( -23.54665576872953636, -14.78900941482413067, -230.7594827126482073 ) ) ;
#6900 = CARTESIAN_POINT ( 'NONE',  ( -20.00523085820573499, 3.356386534894876927, -232.9491364426554298 ) ) ;
#6901 = SURFACE_STYLE_FILL_AREA ( #1822 ) ;
#6902 = CARTESIAN_POINT ( 'NONE',  ( -3.130917144532865848, 26.01013079854885390, -229.4331404728494874 ) ) ;
#6903 = CARTESIAN_POINT ( 'NONE',  ( 20.18206873099720156, 1.748383523995667987, -234.4526011791959661 ) ) ;
#6904 = CIRCLE ( 'NONE', #19462, 3.000000000000033751 ) ;
#6905 = CARTESIAN_POINT ( 'NONE',  ( 21.35706335192880445, 15.67286272432725092, -219.2578158352350783 ) ) ;
#6906 = CARTESIAN_POINT ( 'NONE',  ( 25.40172858355122898, 15.07073195964820833, -229.0276483847865450 ) ) ;
#6907 = CARTESIAN_POINT ( 'NONE',  ( -3.878264816061211651, -12.95777722686681344, -227.3767537598947683 ) ) ;
#6908 = CARTESIAN_POINT ( 'NONE',  ( 2.770531592831002143, 22.28948935999365943, -215.1307751200139649 ) ) ;
#6909 = PRODUCT ( 'Frothing Whisk', 'Frothing Whisk', '', ( #14372 ) ) ;
#6910 = CARTESIAN_POINT ( 'NONE',  ( 16.00819137755116373, 4.595691552992191120, -229.5669508871464757 ) ) ;
#6911 = CARTESIAN_POINT ( 'NONE',  ( 9.903783394593444811, -26.64562852513063973, -229.6560785209296682 ) ) ;
#6912 = CARTESIAN_POINT ( 'NONE',  ( -10.40174557315337900, 22.75579539577861965, -231.4492192189165962 ) ) ;
#6913 = CARTESIAN_POINT ( 'NONE',  ( 2.579827969572558111, 15.91317371615649101, -219.7652087782269916 ) ) ;
#6914 = EDGE_CURVE ( 'NONE', #9939, #9897, #16068, .T. ) ;
#6915 = CARTESIAN_POINT ( 'NONE',  ( -15.58529874627549461, -6.917566422457355202, -219.0138643999995054 ) ) ;
#6916 = CARTESIAN_POINT ( 'NONE',  ( -15.19607346356906952, 9.485739149828241068, -229.2407115334993080 ) ) ;
#6917 = CIRCLE ( 'NONE', #9791, 21.80000000000000071 ) ;
#6918 = CARTESIAN_POINT ( 'NONE',  ( 11.75630001506626776, 9.075791953625659048, -230.4239556728226717 ) ) ;
#6919 = EDGE_LOOP ( 'NONE', ( #16239, #13346, #3996, #7526 ) ) ;
#6920 = CARTESIAN_POINT ( 'NONE',  ( 5.623554730548537606, 15.65270319720736225, -231.3185741195121068 ) ) ;
#6921 = CARTESIAN_POINT ( 'NONE',  ( 26.62161015268053177, -11.01850213254573951, -223.2145259598937344 ) ) ;
#6922 = CARTESIAN_POINT ( 'NONE',  ( 12.31594623278127720, -7.047777776961618557, -228.0736214755532956 ) ) ;
#6923 = PRESENTATION_STYLE_ASSIGNMENT (( #3530 ) ) ;
#6924 = CARTESIAN_POINT ( 'NONE',  ( 22.46220731426537043, 18.23201731183003460, -227.5436199598787539 ) ) ;
#6925 = CARTESIAN_POINT ( 'NONE',  ( -30.11338598929818389, -8.317867968210222784, -227.6364879822423006 ) ) ;
#6926 = CARTESIAN_POINT ( 'NONE',  ( -5.636842872076440081, -13.76003991320737541, -219.7405193562604495 ) ) ;
#6927 = CARTESIAN_POINT ( 'NONE',  ( 5.982950994121768673, -14.58086824529316594, -231.1438280359330975 ) ) ;
#6928 = CARTESIAN_POINT ( 'NONE',  ( -5.706122936196527107, 15.14201253431006045, -228.6865785740211550 ) ) ;
#6929 = EDGE_CURVE ( 'NONE', #20645, #17987, #20687, .T. ) ;
#6930 = CARTESIAN_POINT ( 'NONE',  ( 15.04029996350473830, 7.457450192165341107, -220.5007084872782173 ) ) ;
#6931 = CARTESIAN_POINT ( 'NONE',  ( -25.29098058636142810, 5.014641116111857144, -217.4658967307323110 ) ) ;
#6932 = CARTESIAN_POINT ( 'NONE',  ( -9.060146982536336324, 27.14942986116457746, -225.6568961786626062 ) ) ;
#6933 = CARTESIAN_POINT ( 'NONE',  ( 14.41459438711767760, -7.262430563887544821, -219.0449948566021021 ) ) ;
#6934 = AXIS2_PLACEMENT_3D ( 'NONE', #18621, #12193, #10289 ) ;
#6935 = VECTOR ( 'NONE', #19580, 1000.000000000000000 ) ;
#6936 = CARTESIAN_POINT ( 'NONE',  ( -4.080659539198054020, 15.43130099126780408, -228.8058965243247656 ) ) ;
#6937 = CARTESIAN_POINT ( 'NONE',  ( -26.35007260221545877, 6.140745174321167177, -221.9336216792591188 ) ) ;
#6938 = CARTESIAN_POINT ( 'NONE',  ( 10.85325209735074559, 11.82487774067193342, -216.5214842375702062 ) ) ;
#6939 = CARTESIAN_POINT ( 'NONE',  ( 12.94117841657163126, -3.283311917827119064, -226.8844617769393039 ) ) ;
#6940 = CARTESIAN_POINT ( 'NONE',  ( 0.000000000000000000, 0.000000000000000000, 94.00000000000000000 ) ) ;
#6941 = ORIENTED_EDGE ( 'NONE', *, *, #11715, .F. ) ;
#6942 = CARTESIAN_POINT ( 'NONE',  ( -7.189383125363055349, 14.28512618638020548, -231.7475838278701303 ) ) ;
#6943 = CARTESIAN_POINT ( 'NONE',  ( -10.57293828068126373, -5.503282544971903611, -227.1466070594375708 ) ) ;
#6944 = CYLINDRICAL_SURFACE ( 'NONE', #14100, 23.00000000000008882 ) ;
#6945 = CARTESIAN_POINT ( 'NONE',  ( 27.75679124201660741, 4.911524026080384075, -221.4430403652340829 ) ) ;
#6946 = CARTESIAN_POINT ( 'NONE',  ( -13.98136146596813845, 3.850743984385103680, -228.7620665878280590 ) ) ;
#6947 = CARTESIAN_POINT ( 'NONE',  ( 13.82188917133564132, -5.740199443570373816, -227.9076376976435654 ) ) ;
#6948 = DIRECTION ( 'NONE',  ( 0.000000000000000000, 0.000000000000000000, 1.000000000000000000 ) ) ;
#6949 = CARTESIAN_POINT ( 'NONE',  ( -22.11084984981285118, 10.96048252433489623, -216.6117774006995376 ) ) ;
#6950 = CIRCLE ( 'NONE', #14509, 21.80000000000000071 ) ;
#6951 = CARTESIAN_POINT ( 'NONE',  ( -13.92046207272054303, -0.1600067567908077248, -224.5811699126800818 ) ) ;
#6952 = CARTESIAN_POINT ( 'NONE',  ( 0.2799207934783670693, -28.72270877262613453, -227.3216717588132667 ) ) ;
#6953 = AXIS2_PLACEMENT_3D ( 'NONE', #2293, #3756, #10641 ) ;
#6954 = DIRECTION ( 'NONE',  ( -0.000000000000000000, -0.000000000000000000, -1.000000000000000000 ) ) ;
#6955 = DIRECTION ( 'NONE',  ( -1.000000000000000000, 0.000000000000000000, 0.000000000000000000 ) ) ;
#6956 = CARTESIAN_POINT ( 'NONE',  ( -29.30406754532526037, 5.063969254119831120, -221.8212091093853076 ) ) ;
#6957 = CARTESIAN_POINT ( 'NONE',  ( 16.32467020957917114, -16.75837631771952019, -218.4891864258081853 ) ) ;
#6958 = CARTESIAN_POINT ( 'NONE',  ( 13.58381642412367896, -1.690444079054164161, -222.5208797957015747 ) ) ;
#6959 = CARTESIAN_POINT ( 'NONE',  ( -24.60211427235279302, 4.452209872279524916, 8.960190547743279055 ) ) ;
#6960 = CARTESIAN_POINT ( 'NONE',  ( 10.63406535173453271, 22.16595115341124256, -219.6461356279925781 ) ) ;
#6961 = EDGE_CURVE ( 'NONE', #7178, #18886, #8501, .T. ) ;
#6962 = CARTESIAN_POINT ( 'NONE',  ( -11.19105919052231179, 21.17456633634251872, -216.2128528132037957 ) ) ;
#6963 = CARTESIAN_POINT ( 'NONE',  ( 15.08139719848974103, 12.15862464477973504, -219.3112749338812080 ) ) ;
#6964 = CARTESIAN_POINT ( 'NONE',  ( 5.447232503735224718, -25.66160541809718865, -232.3984543420957323 ) ) ;
#6965 = CARTESIAN_POINT ( 'NONE',  ( 24.23593707391374608, -4.329230177290460446, -233.5551557188744312 ) ) ;
#6966 = CARTESIAN_POINT ( 'NONE',  ( -9.988594796049140356, 11.34066464990972811, -226.6453149279956563 ) ) ;
#6967 = CARTESIAN_POINT ( 'NONE',  ( -15.19607346356906952, 9.485739149828241068, -229.2407115334993080 ) ) ;
#6968 = CARTESIAN_POINT ( 'NONE',  ( -17.18633058961025029, 6.481319267413964802, -216.1357216783315494 ) ) ;
#6969 = VERTEX_POINT ( 'NONE', #1075 ) ;
#6970 = CARTESIAN_POINT ( 'NONE',  ( -3.332878961853828592, -21.58676603248690284, -218.0452238110532619 ) ) ;
#6971 = CARTESIAN_POINT ( 'NONE',  ( -6.539635590297925738, -8.674798497629369720, 92.00000000000001421 ) ) ;
#6972 = AXIS2_PLACEMENT_3D ( 'NONE', #17217, #4711, #20573 ) ;
#6973 = ORIENTED_EDGE ( 'NONE', *, *, #11247, .T. ) ;
#6974 = CARTESIAN_POINT ( 'NONE',  ( 17.76485367938521875, 4.373152267827974171, -218.8623009891758215 ) ) ;
#6975 = CARTESIAN_POINT ( 'NONE',  ( 14.18740332497314149, -14.20295060558812672, -230.7262566610843351 ) ) ;
#6976 = CARTESIAN_POINT ( 'NONE',  ( 4.389496648589924277, 14.47660514356954131, -220.6151178996808540 ) ) ;
#6977 = CARTESIAN_POINT ( 'NONE',  ( -13.83274569775339202, 16.20364235096346661, -234.0851861771356539 ) ) ;
#6978 = CARTESIAN_POINT ( 'NONE',  ( 14.29548763234129538, 2.320071712424730315, -230.2610858871018422 ) ) ;
#6979 = CARTESIAN_POINT ( 'NONE',  ( 5.069241901512100412, 14.34986542013820632, -229.6420000777802954 ) ) ;
#6980 = CARTESIAN_POINT ( 'NONE',  ( 25.18785298611088308, 3.974282393449815931, -218.7636041058819956 ) ) ;
#6981 = CARTESIAN_POINT ( 'NONE',  ( -5.178973235464019886, -24.35492185057628944, -233.6431870320687381 ) ) ;
#6982 = CARTESIAN_POINT ( 'NONE',  ( 13.82188917133564132, -5.740199443570373816, -227.9076376976435654 ) ) ;
#6983 = DIRECTION ( 'NONE',  ( 0.000000000000000000, 0.000000000000000000, -1.000000000000000000 ) ) ;
#6984 = VECTOR ( 'NONE', #15037, 1000.000000000000000 ) ;
#6985 = FACE_OUTER_BOUND ( 'NONE', #16062, .T. ) ;
#6986 = CARTESIAN_POINT ( 'NONE',  ( 28.51464931495100785, 5.422321182929326966, -223.8116416110474347 ) ) ;
#6987 = CARTESIAN_POINT ( 'NONE',  ( -10.41267218490845181, -10.94250683577548244, -225.3448144993165556 ) ) ;
#6988 = CARTESIAN_POINT ( 'NONE',  ( -20.71192633727912380, 6.339941255257877550, -217.2401662359725094 ) ) ;
#6989 = CARTESIAN_POINT ( 'NONE',  ( 3.367418898937407867, 27.20023797116225595, -219.3349021808245709 ) ) ;
#6990 = CARTESIAN_POINT ( 'NONE',  ( 2.482746429915354547, 16.41797261123590346, -229.5599230346982154 ) ) ;
#6991 = ORIENTED_EDGE ( 'NONE', *, *, #19993, .T. ) ;
#6992 = CARTESIAN_POINT ( 'NONE',  ( -25.38303270991942284, -1.762464254583185452, -219.8781034644853776 ) ) ;
#6993 = CARTESIAN_POINT ( 'NONE',  ( 10.07175337281514871, 14.76776740066196325, -231.7834566702614723 ) ) ;
#6994 = CARTESIAN_POINT ( 'NONE',  ( -19.18087294808806931, 21.32275554655070593, -230.8558978902391061 ) ) ;
#6995 = CARTESIAN_POINT ( 'NONE',  ( -16.75232826114664775, 4.232868982398014346, -229.4158550594996200 ) ) ;
#6996 = CARTESIAN_POINT ( 'NONE',  ( -17.90134810484358141, -14.13951559615540710, -232.9640066987647344 ) ) ;
#6997 = FACE_OUTER_BOUND ( 'NONE', #15192, .T. ) ;
#6998 = EDGE_CURVE ( 'NONE', #3746, #8392, #18554, .T. ) ;
#6999 = CARTESIAN_POINT ( 'NONE',  ( 25.62718606866737403, 13.33219119508369310, -230.9315691959737933 ) ) ;
#7000 = STYLED_ITEM ( 'NONE', ( #6923 ), #14295 ) ;
#7001 = CARTESIAN_POINT ( 'NONE',  ( -11.86888352782322897, 15.29489941890347282, -218.1379771575364259 ) ) ;
#7002 = CARTESIAN_POINT ( 'NONE',  ( 17.60070748514786132, 25.68479983175475567, -229.9331108608050158 ) ) ;
#7003 = CARTESIAN_POINT ( 'NONE',  ( 27.16757474806794903, 2.676291341565463888, -220.8863403533574115 ) ) ;
#7004 = CARTESIAN_POINT ( 'NONE',  ( -27.54101393026537181, -2.112662437277116556, -233.6092940012385384 ) ) ;
#7005 = EDGE_LOOP ( 'NONE', ( #9926, #17501, #21095, #13788 ) ) ;
#7006 = CARTESIAN_POINT ( 'NONE',  ( -22.73457989858237127, -6.881456255901889030, -216.4806380023168799 ) ) ;
#7007 = CARTESIAN_POINT ( 'NONE',  ( -10.98447002683091256, 8.146786682930290624, -230.8316952156193338 ) ) ;
#7008 = CARTESIAN_POINT ( 'NONE',  ( 1.292981098121811279, -26.53499626907933262, -232.9055005154886828 ) ) ;
#7009 = CARTESIAN_POINT ( 'NONE',  ( -8.501641725227710111, 25.47064987787527102, -217.3358698761548737 ) ) ;
#7010 = CARTESIAN_POINT ( 'NONE',  ( 13.95236037140391261, -4.360547358326352096, -218.9684814425422132 ) ) ;
#7011 = CARTESIAN_POINT ( 'NONE',  ( 15.27183824227296327, -0.1003146413681868659, -228.0000000000005969 ) ) ;
#7012 = CARTESIAN_POINT ( 'NONE',  ( 20.18206873099720156, 1.748383523995667987, -234.4526011791959661 ) ) ;
#7013 = DIRECTION ( 'NONE',  ( -0.000000000000000000, -0.000000000000000000, 1.000000000000000000 ) ) ;
#7014 = CARTESIAN_POINT ( 'NONE',  ( -3.926352947695993745, 17.69140300707508473, -220.1607884481205986 ) ) ;
#7015 = CARTESIAN_POINT ( 'NONE',  ( 30.47710800431509170, 7.409378661937554789, -223.2007768404241688 ) ) ;
#7016 = CARTESIAN_POINT ( 'NONE',  ( 17.60676319847677007, 21.31475060840986302, -219.8266339603936785 ) ) ;
#7017 = CARTESIAN_POINT ( 'NONE',  ( 17.23039831256031817, 3.331158952577910615, -216.4027685342793461 ) ) ;
#7018 = CARTESIAN_POINT ( 'NONE',  ( -0.1378023845299804762, -12.51091464425689104, -226.1051157421467508 ) ) ;
#7019 = AXIS2_PLACEMENT_3D ( 'NONE', #2348, #14301, #8898 ) ;
#7020 =( GEOMETRIC_REPRESENTATION_CONTEXT ( 3 ) GLOBAL_UNCERTAINTY_ASSIGNED_CONTEXT ( ( #4023 ) ) GLOBAL_UNIT_ASSIGNED_CONTEXT ( ( #4912, #11897, #17080 ) ) REPRESENTATION_CONTEXT ( 'NONE', 'WORKASPACE' ) );
#7021 = CARTESIAN_POINT ( 'NONE',  ( 0.8673818989965740300, 28.69424263383094598, -231.7310846804014659 ) ) ;
#7022 = CARTESIAN_POINT ( 'NONE',  ( 26.00000000000000000, 0.000000000000000000, 0.000000000000000000 ) ) ;
#7023 = CARTESIAN_POINT ( 'NONE',  ( -10.13139158240655391, -23.04245082364802499, -234.6840773296079874 ) ) ;
#7024 = CARTESIAN_POINT ( 'NONE',  ( -10.84440549681320221, 27.00404139634608214, -224.0969657459751261 ) ) ;
#7025 = CARTESIAN_POINT ( 'NONE',  ( 16.69977105456987232, 16.51652889326612694, -233.6667933521891030 ) ) ;
#7026 = CARTESIAN_POINT ( 'NONE',  ( -14.93108815068229589, -1.792787290847115633, -227.6165763581034582 ) ) ;
#7027 = CARTESIAN_POINT ( 'NONE',  ( -16.27736488614644372, 5.941157768540612949, -228.4237983497913547 ) ) ;
#7028 = CARTESIAN_POINT ( 'NONE',  ( -15.54392142943450317, 6.670312097614393920, -219.6934017696036676 ) ) ;
#7030 = CARTESIAN_POINT ( 'NONE',  ( 16.49791052269847569, 3.745513941566326999, -220.1874559167976884 ) ) ;
#7029 = AXIS2_PLACEMENT_3D ( 'NONE', #3784, #2098, #15618 ) ;
#7031 = VERTEX_POINT ( 'NONE', #9414 ) ;
#7032 = CARTESIAN_POINT ( 'NONE',  ( 12.53674998645855787, 17.96979015029927851, -232.8843215672231679 ) ) ;
#7033 = CARTESIAN_POINT ( 'NONE',  ( 9.672299229151310129, -14.28303711772943529, -228.3078296064027484 ) ) ;
#7034 = AXIS2_PLACEMENT_3D ( 'NONE', #20723, #6558, #5304 ) ;
#7035 = ORIENTED_EDGE ( 'NONE', *, *, #21568, .T. ) ;
#7036 = CARTESIAN_POINT ( 'NONE',  ( 13.66858788651615164, -3.112492835348085407, -221.5154270223497690 ) ) ;
#7037 = CARTESIAN_POINT ( 'NONE',  ( -8.316066124693966444, 26.67103469786491843, -222.2304303634109885 ) ) ;
#7038 = ORIENTED_EDGE ( 'NONE', *, *, #955, .F. ) ;
#7039 = CARTESIAN_POINT ( 'NONE',  ( 10.57926812561479757, 10.00910231482511215, -225.8341706491384286 ) ) ;
#7040 = CARTESIAN_POINT ( 'NONE',  ( -11.83854910565153062, -9.589341273415847411, -217.2594489226254098 ) ) ;
#7041 = CARTESIAN_POINT ( 'NONE',  ( -5.279374154171231126, -12.28263746854076466, -222.5283095625445640 ) ) ;
#7042 = CARTESIAN_POINT ( 'NONE',  ( 14.18709644517307922, -11.45356969546147496, -232.2178450427173004 ) ) ;
#7043 = CARTESIAN_POINT ( 'NONE',  ( -0.2748333203896175525, 17.57683079704640505, -221.1444293135629948 ) ) ;
#7044 = LINE ( 'NONE', #11461, #15935 ) ;
#7045 = CARTESIAN_POINT ( 'NONE',  ( 12.56556766396551872, 9.776144415819011613, -223.4791766911294815 ) ) ;
#7046 = CARTESIAN_POINT ( 'NONE',  ( -19.00318367631585659, 13.14621133775862916, -233.8403879275295765 ) ) ;
#7047 = CARTESIAN_POINT ( 'NONE',  ( -7.770318051073092036, 21.02940971564074957, -231.8751410922876630 ) ) ;
#7048 = EDGE_CURVE ( 'NONE', #6170, #4018, #22102, .T. ) ;
#7049 = ORIENTED_EDGE ( 'NONE', *, *, #6067, .T. ) ;
#7050 = CARTESIAN_POINT ( 'NONE',  ( 7.163080459435270164, 24.05253566895842354, -232.4475987112033408 ) ) ;
#7051 = CARTESIAN_POINT ( 'NONE',  ( 17.22423229049764970, 1.395540479540137380, -217.3898520248025363 ) ) ;
#7052 = CARTESIAN_POINT ( 'NONE',  ( 12.75306435971521068, 14.56583715532477186, -214.9711136650476533 ) ) ;
#7053 = CARTESIAN_POINT ( 'NONE',  ( 5.377793152941013233, -17.45375835550001753, -231.2474386379397231 ) ) ;
#7055 = LINE ( 'NONE', #2085, #7143 ) ;
#7054 = VECTOR ( 'NONE', #19206, 1000.000000000000000 ) ;
#7056 = ORIENTED_EDGE ( 'NONE', *, *, #6311, .T. ) ;
#7057 = COLOUR_RGB ( '', 0.09019608, 0.27058824, 0.51372549) ;
#7058 = CARTESIAN_POINT ( 'NONE',  ( -2.698926868850080041, 12.89339462271858316, -226.7595176699009585 ) ) ;
#7059 = CARTESIAN_POINT ( 'NONE',  ( 27.51601410384567359, -3.359424968747257711, -222.6356212526655725 ) ) ;
#7060 = CARTESIAN_POINT ( 'NONE',  ( 0.000000000000000000, 0.000000000000000000, 90.00000000000000000 ) ) ;
#7061 = CARTESIAN_POINT ( 'NONE',  ( 12.71450444683213021, 7.595266944807587350, -224.4213778964231665 ) ) ;
#7062 = CARTESIAN_POINT ( 'NONE',  ( -21.89065952084848021, -0.9940043559354364566, -216.9999999999999716 ) ) ;
#7063 = CARTESIAN_POINT ( 'NONE',  ( 6.131461862964278531, -15.14974102410872625, -231.6805438559109973 ) ) ;
#7064 = CARTESIAN_POINT ( 'NONE',  ( -10.65455960636934662, 10.37188583052882862, -219.5197110153079620 ) ) ;
#7065 = CARTESIAN_POINT ( 'NONE',  ( -20.94800339253696109, 4.477632454355491731, -216.5423208360950298 ) ) ;
#7066 = CARTESIAN_POINT ( 'NONE',  ( 0.9095753368782393267, -25.50589708844611891, -231.1945442011520697 ) ) ;
#7067 = DIRECTION ( 'NONE',  ( 1.000000000000000000, 0.000000000000000000, 0.000000000000000000 ) ) ;
#7068 = CARTESIAN_POINT ( 'NONE',  ( 21.31262902390056624, 0.4111834581965390645, -232.0572713672585792 ) ) ;
#7069 = CARTESIAN_POINT ( 'NONE',  ( -13.11494368899652052, 3.355507568391938200, -225.9121440085824304 ) ) ;
#7070 = CARTESIAN_POINT ( 'NONE',  ( 15.01754996320599744, -10.17932250226635738, -220.3401326760229040 ) ) ;
#7071 = AXIS2_PLACEMENT_3D ( 'NONE', #912, #6309, #1132 ) ;
#7072 = LINE ( 'NONE', #5029, #16750 ) ;
#7073 = LINE ( 'NONE', #14167, #11264 ) ;
#7074 = CARTESIAN_POINT ( 'NONE',  ( 23.24653631066306048, 11.83805845626388020, -219.6020901153134162 ) ) ;
#7075 = CARTESIAN_POINT ( 'NONE',  ( -9.964021556040458805, 12.25789996591640119, -217.8262340283327774 ) ) ;
#7076 = CARTESIAN_POINT ( 'NONE',  ( 23.44063276014420794, 13.61134749381700182, -229.1061940987080732 ) ) ;
#7077 = CARTESIAN_POINT ( 'NONE',  ( 1.792482182455914064, -21.59191373485632681, -217.1959973011389593 ) ) ;
#7078 = CARTESIAN_POINT ( 'NONE',  ( 19.73224149047082321, -2.635265996080750295, -233.5133592171236501 ) ) ;
#7079 = ORIENTED_EDGE ( 'NONE', *, *, #5873, .F. ) ;
#7080 = AXIS2_PLACEMENT_3D ( 'NONE', #20876, #5462, #12344 ) ;
#7081 = CARTESIAN_POINT ( 'NONE',  ( -4.691002462566371101, 21.98518063340150164, -232.2516024630330094 ) ) ;
#7082 = CARTESIAN_POINT ( 'NONE',  ( -22.19349712985372491, 11.03542788991621748, -219.7744882786627443 ) ) ;
#7083 = CARTESIAN_POINT ( 'NONE',  ( -29.50764134580612463, 7.783340782857166573, -219.9768238800827191 ) ) ;
#7084 = ORIENTED_EDGE ( 'NONE', *, *, #6089, .T. ) ;
#7085 = CARTESIAN_POINT ( 'NONE',  ( -10.27880337231260199, -13.06498408352235430, -227.3766186522184682 ) ) ;
#7086 = DIRECTION ( 'NONE',  ( 1.000000000000000000, 0.000000000000000000, 0.000000000000000000 ) ) ;
#7087 = ORIENTED_EDGE ( 'NONE', *, *, #17083, .F. ) ;
#7088 = CARTESIAN_POINT ( 'NONE',  ( 27.50364976068844669, 3.973406265104437729, -228.8805639113908228 ) ) ;
#7089 = CARTESIAN_POINT ( 'NONE',  ( 16.26678737605450564, -16.61684638199339048, -230.8698708339908308 ) ) ;
#7090 = CARTESIAN_POINT ( 'NONE',  ( 14.54149994592679107, 8.070685273005897997, -229.7292930672863349 ) ) ;
#7091 = CARTESIAN_POINT ( 'NONE',  ( -18.39892766464214446, 25.11039525536027739, -225.3444503920457294 ) ) ;
#7092 = EDGE_CURVE ( 'NONE', #3103, #4932, #4125, .T. ) ;
#7093 = CARTESIAN_POINT ( 'NONE',  ( 20.96405783751201213, 6.249056650590980588, -215.6254004080763309 ) ) ;
#7094 = EDGE_CURVE ( 'NONE', #14027, #14742, #8853, .T. ) ;
#7095 = CARTESIAN_POINT ( 'NONE',  ( 15.12287735332712835, 21.03907941686458116, -231.7894952627153202 ) ) ;
#7096 = CARTESIAN_POINT ( 'NONE',  ( 13.39175109400946262, 1.184731213613737566, -222.2403203283322739 ) ) ;
#7097 = EDGE_CURVE ( 'NONE', #20853, #2937, #2011, .T. ) ;
#7098 = CARTESIAN_POINT ( 'NONE',  ( 0.5120693878963755719, -30.63998626839889639, -227.9504769009175220 ) ) ;
#7099 = CARTESIAN_POINT ( 'NONE',  ( 18.22947608839760747, -6.525328669204546905, -217.7409786913911205 ) ) ;
#7100 = CARTESIAN_POINT ( 'NONE',  ( 24.99999999999999645, 1.360023205165816762E-13, -9.000000000000001776 ) ) ;
#7101 = CYLINDRICAL_SURFACE ( 'NONE', #15201, 3.000000000000002665 ) ;
#7102 = CARTESIAN_POINT ( 'NONE',  ( -23.66836017558062011, 21.44695383684080525, -223.6245772351065568 ) ) ;
#7103 = CARTESIAN_POINT ( 'NONE',  ( -15.75487091793989158, -3.404709188850186585, -225.0852311470768825 ) ) ;
#7104 = CARTESIAN_POINT ( 'NONE',  ( 13.06430160593375689, 2.561628050526134182, -220.6026188403641299 ) ) ;
#7105 = CARTESIAN_POINT ( 'NONE',  ( 2.785859284650920031, 14.19821255961969619, -226.9946081512528906 ) ) ;
#7106 = CARTESIAN_POINT ( 'NONE',  ( 0.9879969248128627202, 20.02408072508558945, -218.2055348255049410 ) ) ;
#7107 = EDGE_LOOP ( 'NONE', ( #20848, #8716 ) ) ;
#7108 = CARTESIAN_POINT ( 'NONE',  ( -16.27785121718144623, -3.187812258433146084, -227.1052622255949132 ) ) ;
#7109 = CARTESIAN_POINT ( 'NONE',  ( 18.06016678184731461, 2.257982981100609354, -218.9983079406065940 ) ) ;
#7110 = CARTESIAN_POINT ( 'NONE',  ( -12.30606003331388543, 10.59782772616791036, -231.0021630509705801 ) ) ;
#7111 = CARTESIAN_POINT ( 'NONE',  ( -18.91027996815576628, 5.295101183552822555, -231.2253513302548527 ) ) ;
#7112 = CARTESIAN_POINT ( 'NONE',  ( -13.29422863469367577, -26.11207831950312652, -226.3284374130324750 ) ) ;
#7113 = CARTESIAN_POINT ( 'NONE',  ( -18.71530386740073126, -0.6857509888707814527, -217.6195632122020527 ) ) ;
#7114 = DIRECTION ( 'NONE',  ( 1.000000000000000000, 0.000000000000000000, 0.000000000000000000 ) ) ;
#7115 = CARTESIAN_POINT ( 'NONE',  ( 14.85156906897832485, -2.727936025914895701, -226.2641653400703206 ) ) ;
#7116 = CARTESIAN_POINT ( 'NONE',  ( 0.000000000000000000, 0.000000000000000000, 75.00000000000000000 ) ) ;
#7117 = CARTESIAN_POINT ( 'NONE',  ( -13.92941769543345032, 11.48925904027772127, -219.8938199480626281 ) ) ;
#7118 = CARTESIAN_POINT ( 'NONE',  ( 8.463901354249619757, 8.457277735286822917, -222.5555366599873821 ) ) ;
#7119 = CARTESIAN_POINT ( 'NONE',  ( -20.43618815875133521, 1.403378831510147196, -232.9646741665398224 ) ) ;
#7120 = CARTESIAN_POINT ( 'NONE',  ( -11.89542047990565266, -6.454581786823162304, -219.2692666839191133 ) ) ;
#7121 = EDGE_LOOP ( 'NONE', ( #2766, #19727, #6657, #17242 ) ) ;
#7122 = CARTESIAN_POINT ( 'NONE',  ( -28.09913862414779473, -9.456046895945956265, -221.0065986266286870 ) ) ;
#7123 = CARTESIAN_POINT ( 'NONE',  ( -7.352050649209116884, 10.05454564170545417, -223.7370967983176229 ) ) ;
#7124 = CARTESIAN_POINT ( 'NONE',  ( -7.832594822155400927, -23.57318293858060088, -216.4298491688572028 ) ) ;
#7125 = CARTESIAN_POINT ( 'NONE',  ( 9.107417252317809186, 16.30291009569977234, -218.0131178633739921 ) ) ;
#7126 = CARTESIAN_POINT ( 'NONE',  ( 7.144703960786618957, -9.913249271193393497, -228.5244988832443198 ) ) ;
#7127 = CARTESIAN_POINT ( 'NONE',  ( 0.000000000000000000, 0.000000000000000000, -78.50000000000000000 ) ) ;
#7128 = CARTESIAN_POINT ( 'NONE',  ( 17.34461553379066601, 6.893916422670210764, -233.3442385185644525 ) ) ;
#7129 = DIRECTION ( 'NONE',  ( -0.000000000000000000, -0.000000000000000000, 1.000000000000000000 ) ) ;
#7130 = PRODUCT_DEFINITION ( 'UNKNOWN', '', #8511, #21564 ) ;
#7131 = CARTESIAN_POINT ( 'NONE',  ( -2.723069588102707606, 15.58614045890443833, -225.0254611642426141 ) ) ;
#7132 = CARTESIAN_POINT ( 'NONE',  ( -17.43458823433387650, 2.804998135793385750, -231.8077100320880959 ) ) ;
#7133 = CARTESIAN_POINT ( 'NONE',  ( 21.39553407250273054, 8.453402029343234148, -217.9531594780983141 ) ) ;
#7134 = CARTESIAN_POINT ( 'NONE',  ( 13.98152565379061052, 2.156981915107639036, -230.5667344709999611 ) ) ;
#7135 = CARTESIAN_POINT ( 'NONE',  ( -3.535116539333309049, -19.81104435003528152, -216.2789031305144931 ) ) ;
#7136 = CARTESIAN_POINT ( 'NONE',  ( 8.126072675580726212, 14.68573014611672534, -233.8823376361746966 ) ) ;
#7137 = DIRECTION ( 'NONE',  ( 0.000000000000000000, 0.000000000000000000, -1.000000000000000000 ) ) ;
#7138 = CARTESIAN_POINT ( 'NONE',  ( -15.15491452760745439, -27.84330619910961957, -221.4571841043341180 ) ) ;
#7139 = CARTESIAN_POINT ( 'NONE',  ( -4.879985665934096772, 15.33285679834440174, -220.9402849574511833 ) ) ;
#7140 = CARTESIAN_POINT ( 'NONE',  ( 11.63337745479824292, 8.229076005436313679, -220.5472098800687206 ) ) ;
#7141 = CARTESIAN_POINT ( 'NONE',  ( -15.15819830826754355, -2.370657588173597841, -221.8013720140894236 ) ) ;
#7142 = CARTESIAN_POINT ( 'NONE',  ( -16.88145396433676027, 5.002512658926777434, -221.2364783498041731 ) ) ;
#7143 = VECTOR ( 'NONE', #5679, 1000.000000000000000 ) ;
#7144 = CARTESIAN_POINT ( 'NONE',  ( -4.296082356836364191, 12.57880442405704002, -229.5247240216588125 ) ) ;
#7145 = CARTESIAN_POINT ( 'NONE',  ( 18.55287065739596031, 7.869864349944380777, -232.8430408253643691 ) ) ;
#7146 = ORIENTED_EDGE ( 'NONE', *, *, #19953, .T. ) ;
#7147 = CARTESIAN_POINT ( 'NONE',  ( 13.43702744235484303, -16.51261215982735209, -219.1853238157515875 ) ) ;
#7148 = CARTESIAN_POINT ( 'NONE',  ( 4.804712767000853368, -14.77773536573586455, -228.5128529893618747 ) ) ;
#7149 = APPLICATION_CONTEXT ( 'automotive_design' ) ;
#7150 = CARTESIAN_POINT ( 'NONE',  ( -5.560972518124746244, 14.60655266358653215, -227.5460946431043681 ) ) ;
#7151 = CARTESIAN_POINT ( 'NONE',  ( 0.000000000000000000, 25.00000000000000000, -75.00000000000000000 ) ) ;
#7152 = CARTESIAN_POINT ( 'NONE',  ( 21.35706335192880445, 15.67286272432725092, -219.2578158352350783 ) ) ;
#7153 = CARTESIAN_POINT ( 'NONE',  ( 27.32546652195855685, -7.354568365469916991, -229.0866163655393279 ) ) ;
#7154 = CARTESIAN_POINT ( 'NONE',  ( -13.21314811618155716, -9.038438575223175064, -230.6430079410957603 ) ) ;
#7155 = CARTESIAN_POINT ( 'NONE',  ( -1.778254167844783851, -12.78790610364390012, -225.9413532495922254 ) ) ;
#7156 = CARTESIAN_POINT ( 'NONE',  ( -2.906906946766868227, 27.66682465340607422, -226.6559963821499082 ) ) ;
#7157 = DIRECTION ( 'NONE',  ( 0.000000000000000000, 0.000000000000000000, 1.000000000000000000 ) ) ;
#7158 = CARTESIAN_POINT ( 'NONE',  ( 14.03916608299427082, 11.26328028684000415, -220.2447382113059007 ) ) ;
#7159 = CARTESIAN_POINT ( 'NONE',  ( -11.69688825528096388, 18.63404371591177622, -215.8612738028812714 ) ) ;
#7160 = CARTESIAN_POINT ( 'NONE',  ( -16.90193019167508126, 18.45790510038867893, -217.5707532411249758 ) ) ;
#7161 = CARTESIAN_POINT ( 'NONE',  ( 4.303123380281038024, 17.66787810618728827, -231.9745698734655832 ) ) ;
#7162 = CARTESIAN_POINT ( 'NONE',  ( -18.46822229429615447, 3.027586163204024405, -230.1002726880134333 ) ) ;
#7163 = CARTESIAN_POINT ( 'NONE',  ( 6.812728368504421539, 14.35307019806973194, -216.7766581591129977 ) ) ;
#7164 = CIRCLE ( 'NONE', #19005, 5.500000000000000000 ) ;
#7165 = CARTESIAN_POINT ( 'NONE',  ( 12.70013114424463296, -16.94540864491495924, -217.3462533088837745 ) ) ;
#7166 = DIRECTION ( 'NONE',  ( -1.000000000000000000, 0.000000000000000000, 0.000000000000000000 ) ) ;
#7167 = ORIENTED_EDGE ( 'NONE', *, *, #15545, .T. ) ;
#7168 = ADVANCED_FACE ( 'NONE', ( #3615 ), #15680, .T. ) ;
#7169 = CARTESIAN_POINT ( 'NONE',  ( -8.823862513872974489, 14.92351368520778898, -217.1499513473673346 ) ) ;
#7170 = CARTESIAN_POINT ( 'NONE',  ( -32.13037437807204810, -1.025156162654832670, -224.7589498746283141 ) ) ;
#7171 = CARTESIAN_POINT ( 'NONE',  ( 17.00614511541963836, -1.958782916976874233, -219.4638360731791806 ) ) ;
#7172 = CARTESIAN_POINT ( 'NONE',  ( 23.49048926389013658, 9.645778135078892035, -218.7307869890797463 ) ) ;
#7173 = CARTESIAN_POINT ( 'NONE',  ( -15.23434562258889891, -0.4010941804143903222, -220.4743703065900036 ) ) ;
#7174 = CARTESIAN_POINT ( 'NONE',  ( 14.99336262864975211, -23.54026314425397004, -231.3018640253376361 ) ) ;
#7175 = DIRECTION ( 'NONE',  ( 1.000000000000000000, 0.000000000000000000, 0.000000000000000000 ) ) ;
#7176 = CARTESIAN_POINT ( 'NONE',  ( -10.24288955603410933, 28.30762631303078791, -220.8855665231519083 ) ) ;
#7177 = CARTESIAN_POINT ( 'NONE',  ( -17.20794623181132721, 21.97849129791581291, -217.9187454682870850 ) ) ;
#7178 = VERTEX_POINT ( 'NONE', #20830 ) ;
#7179 = CARTESIAN_POINT ( 'NONE',  ( -26.02440924314744919, 2.824604386891162111, -232.0644005296583430 ) ) ;
#7180 = CARTESIAN_POINT ( 'NONE',  ( -14.34029329777712469, -14.57793623142476669, -217.2545494607695389 ) ) ;
#7181 = CARTESIAN_POINT ( 'NONE',  ( 0.000000000000000000, 0.000000000000000000, -99.99999999999998579 ) ) ;
#7182 = CARTESIAN_POINT ( 'NONE',  ( 23.06814834742187514, -2.825033403592650701E-15, -74.48236190979496030 ) ) ;
#7183 = CARTESIAN_POINT ( 'NONE',  ( -20.94800339253696109, 4.477632454355491731, -216.5423208360950298 ) ) ;
#7184 = CARTESIAN_POINT ( 'NONE',  ( 3.489817674839083228, -23.52381883976217836, -233.5393804659674117 ) ) ;
#7185 = CARTESIAN_POINT ( 'NONE',  ( -23.33862492659004317, 8.963030688957390524, 4.446446727170273228 ) ) ;
#7186 = CARTESIAN_POINT ( 'NONE',  ( 14.72648027392381387, 10.15511732729369676, -229.5776536674053716 ) ) ;
#7187 = CARTESIAN_POINT ( 'NONE',  ( -16.38161496430853248, 17.22219235543852989, -215.3343469598664797 ) ) ;
#7188 = CARTESIAN_POINT ( 'NONE',  ( 22.03647168421188596, 0.3315607655626346961, -232.0572713672587213 ) ) ;
#7189 = CARTESIAN_POINT ( 'NONE',  ( 14.03916608299427082, 11.26328028684000415, -220.2447382113059007 ) ) ;
#7190 = CARTESIAN_POINT ( 'NONE',  ( 3.550474435626596037, -26.82390172985419952, -218.7255222707324549 ) ) ;
#7191 = CARTESIAN_POINT ( 'NONE',  ( 14.01369322398082851, -0.3099216430074364093, -221.6784101578248283 ) ) ;
#7192 = ORIENTED_EDGE ( 'NONE', *, *, #3073, .T. ) ;
#7193 = CARTESIAN_POINT ( 'NONE',  ( -5.775873073292457249, 17.47547275616994256, -218.7209647771908578 ) ) ;
#7194 = CARTESIAN_POINT ( 'NONE',  ( -21.99356461413155728, 5.827088221545293045, -219.1725956997024127 ) ) ;
#7195 = CARTESIAN_POINT ( 'NONE',  ( 16.55609572527610851, 2.729108819536508967, -230.5704679660131831 ) ) ;
#7196 = VERTEX_POINT ( 'NONE', #19369 ) ;
#7197 = CARTESIAN_POINT ( 'NONE',  ( -18.43493186415240714, -20.29552032882516244, -227.2236339120829030 ) ) ;
#7198 = DIRECTION ( 'NONE',  ( 0.000000000000000000, 0.000000000000000000, -1.000000000000000000 ) ) ;
#7199 = ORIENTED_EDGE ( 'NONE', *, *, #11762, .T. ) ;
#7200 = CARTESIAN_POINT ( 'NONE',  ( 18.78616100366561881, 3.045752412654093355, -231.5393376370170699 ) ) ;
#7201 = CARTESIAN_POINT ( 'NONE',  ( 8.483411394722875087, -26.22410139474833457, -227.7697325675642617 ) ) ;
#7202 = CARTESIAN_POINT ( 'NONE',  ( 16.38151749656409351, 8.902090001712490874, -231.2955017965201989 ) ) ;
#7203 = CARTESIAN_POINT ( 'NONE',  ( -8.823862513872974489, 14.92351368520778898, -217.1499513473673346 ) ) ;
#7204 = CARTESIAN_POINT ( 'NONE',  ( 29.33969601628096768, 11.98971187598327504, -225.2039690377576733 ) ) ;
#7205 = EDGE_CURVE ( 'NONE', #19105, #324, #9148, .T. ) ;
#7206 = CARTESIAN_POINT ( 'NONE',  ( 9.107417252317809186, 16.30291009569977234, -218.0131178633739921 ) ) ;
#7207 = DIRECTION ( 'NONE',  ( -1.000000000000000000, 0.000000000000000000, 0.000000000000000000 ) ) ;
#7208 = CARTESIAN_POINT ( 'NONE',  ( -10.11868820210310282, -13.51996935893276053, -218.1704188629865371 ) ) ;
#7209 = CARTESIAN_POINT ( 'NONE',  ( 12.70477135646371281, -9.814387909761604689, -230.3443492180780652 ) ) ;
#7210 = FACE_OUTER_BOUND ( 'NONE', #11890, .T. ) ;
#7211 = DIRECTION ( 'NONE',  ( -1.000000000000000000, 0.000000000000000000, 0.000000000000000000 ) ) ;
#7212 = CARTESIAN_POINT ( 'NONE',  ( -27.53108621362071773, 14.15137273650544536, -219.7961709676081625 ) ) ;
#7213 = CARTESIAN_POINT ( 'NONE',  ( 22.16968511661848495, 1.542591969257128826, -234.6098499860488857 ) ) ;
#7214 = EDGE_CURVE ( 'NONE', #161, #7856, #14609, .T. ) ;
#7215 = CARTESIAN_POINT ( 'NONE',  ( 28.53243699394185384, 6.329221954355706004, -218.6437889135959267 ) ) ;
#7216 = CARTESIAN_POINT ( 'NONE',  ( 5.702651035983461902, 12.42242820409033222, -224.7304266323218656 ) ) ;
#7217 = CARTESIAN_POINT ( 'NONE',  ( 5.365126951644291431, 19.60085171667039816, -218.9155869426879519 ) ) ;
#7218 = ORIENTED_EDGE ( 'NONE', *, *, #20925, .F. ) ;
#7219 = CARTESIAN_POINT ( 'NONE',  ( 9.772444363920737231, -9.146208674228628155, -219.7841758423534486 ) ) ;
#7220 = ORIENTED_EDGE ( 'NONE', *, *, #14341, .T. ) ;
#7221 = CARTESIAN_POINT ( 'NONE',  ( 14.98418162551161714, 4.450317369940187895, -227.9894155827521161 ) ) ;
#7222 = CARTESIAN_POINT ( 'NONE',  ( -14.95675039876920032, 11.42095949000369259, -217.2220932760075129 ) ) ;
#7223 = CARTESIAN_POINT ( 'NONE',  ( -10.95054816480499760, 8.339404316518379545, -224.1596700080921778 ) ) ;
#7224 = CARTESIAN_POINT ( 'NONE',  ( -14.80115690555879659, -8.758261077448048937, -218.2925738755452016 ) ) ;
#7225 = CARTESIAN_POINT ( 'NONE',  ( -15.58461825850822180, 18.91734573546571951, -233.7691177939990723 ) ) ;
#7226 = DIRECTION ( 'NONE',  ( -1.000000000000000000, 0.000000000000000000, 0.000000000000000000 ) ) ;
#7227 = CARTESIAN_POINT ( 'NONE',  ( 25.50000000000000000, 0.000000000000000000, 0.000000000000000000 ) ) ;
#7228 = CARTESIAN_POINT ( 'NONE',  ( 13.19406830060760605, 4.163358546877222288, -228.8532745215267425 ) ) ;
#7229 = CARTESIAN_POINT ( 'NONE',  ( -12.33583941212908108, 22.27382123621224608, -231.6290720151527296 ) ) ;
#7230 = CARTESIAN_POINT ( 'NONE',  ( 19.13589083395335422, 16.69125564174534659, -234.7442498487877174 ) ) ;
#7231 = CARTESIAN_POINT ( 'NONE',  ( -13.65925618638770800, 3.289586759644148817, -222.1579143493116533 ) ) ;
#7232 = CARTESIAN_POINT ( 'NONE',  ( -14.04855893775563125, -7.839533416607601168, -216.6740050463540115 ) ) ;
#7233 = CARTESIAN_POINT ( 'NONE',  ( -30.71739798481564421, -2.702902032605977389, -225.9472362185736642 ) ) ;
#7234 = CARTESIAN_POINT ( 'NONE',  ( -17.81561310496929806, 18.25637658208611569, -215.7745954696244439 ) ) ;
#7235 = CARTESIAN_POINT ( 'NONE',  ( -8.257247207528708444, -26.39349301559143512, -217.9383130379005138 ) ) ;
#7236 = CARTESIAN_POINT ( 'NONE',  ( 8.329997790135040603, 12.51216704542961899, -228.7022893680961602 ) ) ;
#7237 = CARTESIAN_POINT ( 'NONE',  ( 12.91141610427636621, -26.43280511468161720, -217.7946055251781274 ) ) ;
#7238 = CARTESIAN_POINT ( 'NONE',  ( 26.00000000000000000, 3.600000000000000533, -2.700000000000000622 ) ) ;
#7239 = CARTESIAN_POINT ( 'NONE',  ( -20.71192633727912380, 6.339941255257877550, -217.2401662359725094 ) ) ;
#7240 = CARTESIAN_POINT ( 'NONE',  ( 0.000000000000000000, 0.000000000000000000, -75.00000000000000000 ) ) ;
#7241 = CARTESIAN_POINT ( 'NONE',  ( 1.455106383990497187, 21.12056149333958999, -230.8076663600630241 ) ) ;
#7242 = CARTESIAN_POINT ( 'NONE',  ( -22.10934047915427314, 0.9940043559354312386, -216.9999999999999716 ) ) ;
#7243 = CARTESIAN_POINT ( 'NONE',  ( 25.33562512631297281, 12.25422971834577268, -228.6777356031426791 ) ) ;
#7244 = CARTESIAN_POINT ( 'NONE',  ( 11.54460987479198053, 9.649171130674412566, -228.7280371210653698 ) ) ;
#7245 = CARTESIAN_POINT ( 'NONE',  ( -9.447593206125553422, -28.82180577676834332, -226.7547558591687675 ) ) ;
#7246 = CARTESIAN_POINT ( 'NONE',  ( 8.036750260989780514, 26.29729070384984624, -233.5018314387838529 ) ) ;
#7247 = DIRECTION ( 'NONE',  ( 0.000000000000000000, 0.000000000000000000, -1.000000000000000000 ) ) ;
#7248 = CARTESIAN_POINT ( 'NONE',  ( -4.912481909026474192, -29.12074637257241250, -231.0965163926508410 ) ) ;
#7249 = CARTESIAN_POINT ( 'NONE',  ( -4.067324790461362305, 15.10342260507846746, -228.2464404076259257 ) ) ;
#7250 = CARTESIAN_POINT ( 'NONE',  ( 16.55626903245587656, 22.80423546114836952, -218.9884947126587633 ) ) ;
#7251 = CARTESIAN_POINT ( 'NONE',  ( -13.58070052954164275, 11.19572749768420650, -220.2511552028196604 ) ) ;
#7252 = CARTESIAN_POINT ( 'NONE',  ( -7.403072389817287657, 18.92851032520892929, -215.2068968469505137 ) ) ;
#7253 = CARTESIAN_POINT ( 'NONE',  ( 16.56146809408446430, -0.9616313295950813522, -228.5729530379900609 ) ) ;
#7254 = VERTEX_POINT ( 'NONE', #14218 ) ;
#7255 = CARTESIAN_POINT ( 'NONE',  ( 9.923626285694149729, -13.24753681723166210, -222.8613851586638361 ) ) ;
#7256 = ORIENTED_EDGE ( 'NONE', *, *, #13528, .F. ) ;
#7257 = CARTESIAN_POINT ( 'NONE',  ( 9.759123193367146953, -21.89695672029116480, -217.8292787338521919 ) ) ;
#7258 = CARTESIAN_POINT ( 'NONE',  ( -7.366083718505351818, 19.86648438590005838, -231.8662444779758971 ) ) ;
#7259 = ORIENTED_EDGE ( 'NONE', *, *, #627, .T. ) ;
#7260 =( NAMED_UNIT ( * ) SI_UNIT ( $, .STERADIAN. ) SOLID_ANGLE_UNIT ( ) );
#7261 = VECTOR ( 'NONE', #10925, 1000.000000000000000 ) ;
#7262 = CARTESIAN_POINT ( 'NONE',  ( 17.43816562714825125, 15.15720016074785903, -232.3748236813696906 ) ) ;
#7263 = CARTESIAN_POINT ( 'NONE',  ( 27.36047156164216787, -8.591464759722228450, -221.3690063136810977 ) ) ;
#7264 = CARTESIAN_POINT ( 'NONE',  ( -12.04756914620937636, -13.80987496524771885, -232.8991007102355582 ) ) ;
#7265 = CARTESIAN_POINT ( 'NONE',  ( 4.682724365302521896, -22.35092628325669750, -215.9543778044225348 ) ) ;
#7266 = CARTESIAN_POINT ( 'NONE',  ( 0.6289891638115701067, 16.47510600144228832, -227.0521699048171342 ) ) ;
#7267 = DIRECTION ( 'NONE',  ( -1.000000000000000000, 0.000000000000000000, -0.000000000000000000 ) ) ;
#7268 = CARTESIAN_POINT ( 'NONE',  ( 12.51085646230496273, 9.582567546749562126, -224.6200301875240939 ) ) ;
#7269 = ADVANCED_FACE ( 'NONE', ( #10493 ), #13884, .F. ) ;
#7270 = CARTESIAN_POINT ( 'NONE',  ( -2.817219543927646175, 14.13981714106644993, -229.6779615865167443 ) ) ;
#7271 = CARTESIAN_POINT ( 'NONE',  ( -13.30451247859013897, 19.85560227862636040, -232.3493821534129609 ) ) ;
#7272 = ORIENTED_EDGE ( 'NONE', *, *, #21646, .T. ) ;
#7273 = VECTOR ( 'NONE', #1426, 1000.000000000000000 ) ;
#7274 = CARTESIAN_POINT ( 'NONE',  ( 3.080453011304693511, 29.32691491905673331, -222.8956499783474499 ) ) ;
#7275 = CARTESIAN_POINT ( 'NONE',  ( -16.04492519386327487, 1.819644280589142626, -223.4665098021627614 ) ) ;
#7276 = CARTESIAN_POINT ( 'NONE',  ( 22.17049319811867036, 0.5483778423327810847, -216.5715983009590673 ) ) ;
#7277 = CARTESIAN_POINT ( 'NONE',  ( 6.203932113039332563, -21.09630782756332223, -232.3325312104709894 ) ) ;
#7278 = CARTESIAN_POINT ( 'NONE',  ( 17.57135037026572277, 0.09191994211922807634, -232.8447871904542410 ) ) ;
#7279 = ORIENTED_EDGE ( 'NONE', *, *, #14581, .T. ) ;
#7280 = CARTESIAN_POINT ( 'NONE',  ( 4.603870848087811218, 30.13529352683433515, -225.9623629403671430 ) ) ;
#7281 = CARTESIAN_POINT ( 'NONE',  ( 17.02517607141322031, -4.660589389729973497, -229.0519452290894833 ) ) ;
#7282 = CARTESIAN_POINT ( 'NONE',  ( 0.000000000000000000, 0.000000000000000000, 78.50000000000000000 ) ) ;
#7283 = TOROIDAL_SURFACE ( 'NONE', #1155, 24.63401512838761320, 3.000000000000035083 ) ;
#7284 = CARTESIAN_POINT ( 'NONE',  ( 16.64225601860865211, 1.926018578292457928, -220.2177910260893725 ) ) ;
#7285 = CARTESIAN_POINT ( 'NONE',  ( 2.098184199980985376, -13.29281380427311099, -222.1652846463370281 ) ) ;
#7286 =( LENGTH_UNIT ( ) NAMED_UNIT ( * ) SI_UNIT ( .MILLI., .METRE. ) );
#7287 = CARTESIAN_POINT ( 'NONE',  ( -22.04257564474043818, 18.72061943465525857, -219.1781831295219263 ) ) ;
#7288 = CARTESIAN_POINT ( 'NONE',  ( -8.995433708001568718, 13.44373928221519243, -231.9251680978426577 ) ) ;
#7289 = CARTESIAN_POINT ( 'NONE',  ( -18.71530386740073126, -0.6857509888707814527, -217.6195632122020527 ) ) ;
#7290 = CARTESIAN_POINT ( 'NONE',  ( -14.80115690555879659, -8.758261077448048937, -218.2925738755452016 ) ) ;
#7291 = DIRECTION ( 'NONE',  ( 1.000000000000000000, 0.000000000000000000, 0.000000000000000000 ) ) ;
#7292 = LINE ( 'NONE', #15734, #5944 ) ;
#7293 = CARTESIAN_POINT ( 'NONE',  ( -28.59157645096996347, 5.137867505054540374, -220.4667042235044505 ) ) ;
#7294 = CARTESIAN_POINT ( 'NONE',  ( 4.343570314325058135, -14.31236505836544026, -220.3716640818165615 ) ) ;
#7295 = AXIS2_PLACEMENT_3D ( 'NONE', #5618, #12496, #15533 ) ;
#7296 = CARTESIAN_POINT ( 'NONE',  ( -22.94872826613853434, 9.917518390247439086, 1.324323043557437574 ) ) ;
#7297 = EDGE_CURVE ( 'NONE', #862, #19977, #17477, .T. ) ;
#7298 = CARTESIAN_POINT ( 'NONE',  ( 24.38255093784924199, 7.851200578213498815, -231.2687759850219607 ) ) ;
#7299 = CARTESIAN_POINT ( 'NONE',  ( -6.331039912586185814, 17.62337457105953220, -233.2305561356360499 ) ) ;
#7300 = LINE ( 'NONE', #7624, #15934 ) ;
#7301 = CARTESIAN_POINT ( 'NONE',  ( 11.05872493453861161, 12.09300746323778775, -226.7727269015348952 ) ) ;
#7302 = CARTESIAN_POINT ( 'NONE',  ( 0.2144678239183100965, -16.00554277676860693, -220.6792656679080267 ) ) ;
#7303 = VERTEX_POINT ( 'NONE', #371 ) ;
#7304 = CARTESIAN_POINT ( 'NONE',  ( -0.1881941282075867139, 17.37563936270229092, -230.9177995227891813 ) ) ;
#7305 = CARTESIAN_POINT ( 'NONE',  ( -9.523248388595575875, 12.31121908620753125, -221.6288572946744182 ) ) ;
#7306 = CARTESIAN_POINT ( 'NONE',  ( -12.88152464663890306, 6.317716727793897924, -230.5294309895745073 ) ) ;
#7307 = CARTESIAN_POINT ( 'NONE',  ( -13.72210242120180901, -11.34614737046836908, -229.0742334187831659 ) ) ;
#7308 = DIRECTION ( 'NONE',  ( -1.000000000000000000, 0.000000000000000000, 0.000000000000000000 ) ) ;
#7309 = VERTEX_POINT ( 'NONE', #7238 ) ;
#7310 = CARTESIAN_POINT ( 'NONE',  ( 19.87150736056128864, 8.436445599727830924, -233.0166429845654932 ) ) ;
#7311 = CARTESIAN_POINT ( 'NONE',  ( 6.900253619295916963, -14.54306101932516881, -223.7596260804713211 ) ) ;
#7312 = CARTESIAN_POINT ( 'NONE',  ( 24.42567939027770407, 10.22651298688739097, -219.4562066833365748 ) ) ;
#7313 = CARTESIAN_POINT ( 'NONE',  ( -9.749377714296398878, 10.28442384816749922, -229.3722863967025205 ) ) ;
#7314 = CIRCLE ( 'NONE', #16629, 19.00000000000000711 ) ;
#7315 = AXIS2_PLACEMENT_3D ( 'NONE', #885, #665, #16199 ) ;
#7316 = CARTESIAN_POINT ( 'NONE',  ( 12.48419387172699579, 6.663456953110941328, -219.2717027540951165 ) ) ;
#7317 = CARTESIAN_POINT ( 'NONE',  ( 4.543450689403089271, 15.91052110650461771, -218.9437823786444426 ) ) ;
#7318 = CARTESIAN_POINT ( 'NONE',  ( 0.000000000000000000, 0.000000000000000000, -120.0000000000000142 ) ) ;
#7319 = CARTESIAN_POINT ( 'NONE',  ( -5.902479482706956659, -14.78727544128710214, -218.5565286504736946 ) ) ;
#7320 = CARTESIAN_POINT ( 'NONE',  ( 13.62757736989142465, -5.584028114184929947, -227.2616851496390211 ) ) ;
#7321 = ADVANCED_FACE ( 'NONE', ( #12410 ), #16397, .T. ) ;
#7322 = CARTESIAN_POINT ( 'NONE',  ( 25.50000000000000000, 0.000000000000000000, 0.000000000000000000 ) ) ;
#7323 = DIRECTION ( 'NONE',  ( -0.000000000000000000, -0.000000000000000000, -1.000000000000000000 ) ) ;
#7324 = CARTESIAN_POINT ( 'NONE',  ( -21.50655177804914686, 20.61731362457859973, -218.7935603611527426 ) ) ;
#7325 = CARTESIAN_POINT ( 'NONE',  ( -24.13290183362846264, -6.995619630784887022, -220.0347092962472288 ) ) ;
#7326 = CIRCLE ( 'NONE', #4417, 23.00000000000000000 ) ;
#7327 = AXIS2_PLACEMENT_3D ( 'NONE', #19087, #5133, #18874 ) ;
#7328 = CARTESIAN_POINT ( 'NONE',  ( -13.88743542672353826, 10.36310385030668613, -230.6144170796622745 ) ) ;
#7329 = CARTESIAN_POINT ( 'NONE',  ( 11.09231067055629616, 7.417581979752235100, -227.5152062457793534 ) ) ;
#7330 = CARTESIAN_POINT ( 'NONE',  ( -1.268862717067444024, 15.25222216985846480, -229.0661283592426116 ) ) ;
#7331 = VERTEX_POINT ( 'NONE', #19262 ) ;
#7332 = CARTESIAN_POINT ( 'NONE',  ( 11.85708236628466672, -10.49065743416967145, -217.1712987709648530 ) ) ;
#7333 = VERTEX_POINT ( 'NONE', #17588 ) ;
#7334 = CARTESIAN_POINT ( 'NONE',  ( 21.60524407607017849, 3.028118258437591415, -217.8361640396714449 ) ) ;
#7335 = ADVANCED_FACE ( 'NONE', ( #12628, #2154 ), #9034, .F. ) ;
#7336 = CARTESIAN_POINT ( 'NONE',  ( -19.58639255110637478, 14.91076398872931819, -217.1105532241463720 ) ) ;
#7337 = CARTESIAN_POINT ( 'NONE',  ( -11.27928845652762213, 14.86256579634383002, -216.2427993537644966 ) ) ;
#7338 = CARTESIAN_POINT ( 'NONE',  ( -24.95227886253013239, -16.82584358170602101, -223.8363818545792299 ) ) ;
#7339 = CARTESIAN_POINT ( 'NONE',  ( -14.00380962569832199, 8.747390586476997854, -231.7950903513155936 ) ) ;
#7340 = LINE ( 'NONE', #3939, #7631 ) ;
#7341 = CARTESIAN_POINT ( 'NONE',  ( 29.11492790716816614, 6.132849117128307270, -229.8316941169402412 ) ) ;
#7342 = VECTOR ( 'NONE', #4681, 1000.000000000000000 ) ;
#7343 = CARTESIAN_POINT ( 'NONE',  ( -12.14452111807825041, 26.21581784948545035, -221.1455569020914140 ) ) ;
#7344 = CARTESIAN_POINT ( 'NONE',  ( 23.07558131619435571, 16.33594519118144817, -217.0553921114837124 ) ) ;
#7345 = CARTESIAN_POINT ( 'NONE',  ( 17.47660375112063491, 0.1533180678384444551, -220.6249646429494931 ) ) ;
#7346 = B_SPLINE_CURVE_WITH_KNOTS ( 'NONE', 3,
 ( #15023, #18506, #6343, #7113, #1284, #20817, #21973, #3602, #6452, #11522, #1170, #18284, #9956, #20279, #2955, #16815, #15251, #4874, #1921, #8802, #1391, #9843, #16589, #11753, #16704, #8158, #8381, #14914, #21753, #15663, #13216, #18619, #13322, #20163, #4756, #10064, #16928, #6686, #20393, #5289, #12168, #244, #5735, #3711, #17796, #7665, #5632, #15884, #2142, #19459, #3938, #12509, #2362, #5517, #9352, #462, #9020, #19572, #19356, #3827, #10813, #7447, #17681, #14090, #9132, #2252, #4048, #15778, #7339, #9246, #14535, #17573, #12396, #14206, #16212, #17906, #4159, #10924, #21370, #17463, #15995, #2470, #19247, #19131, #10594, #14421, #16106, #2033, #678, #21042, #8912, #571, #14315, #21147, #784, #12279, #7553, #358, #12614, #7225, #21254, #12726, #5846, #11040, #20930, #10709, #4599, #4268, #1235, #13168, #1347, #6178, #1011, #11583, #16768, #3020, #2692, #13275, #6294, #18238, #11146, #2904, #1119, #18457, #20118, #21589, #15090, #13057, #4706, #899, #12838, #19902, #19682, #18014, #9905, #6071, #16654, #9789, #11255, #11476, #2580, #5961, #20013, #8218, #16437, #11369, #2799, #8109, #9463, #16323, #21477, #7995, #21816, #19788, #7777, #14975, #7886, #14646, #12943, #9574, #18343, #18125, #4371, #4490, #14748, #9681, #16540, #14860, #6405, #21703, #4824, #3135, #10016, #18681, #18788, #8446, #17212, #8780, #12146, #6516, #105, #13847, #13728, #1895, #11701, #20457, #15199, #6860, #13619, #10239, #10458, #6976, #16992, #18571, #5156, #3581, #20342, #13385, #21926, #22045, #15422, #18897, #17319, #5045, #1455, #15315, #16880, #6634, #8328, #4938, #20229, #19002, #20568, #12036, #16407, #15522, #1574, #13505, #11814, #3243, #8558, #20684, #10127, #11922, #3471, #22162, #3356, #6751, #17105, #1684, #10349, #1786, #8661, #5266, #12701, #7424, #14293, #15973, #9222, #10688, #5373, #19224, #2225, #547, #15755, #12488, #19108, #5490, #3685, #19335, #12257, #13957, #5822, #12374, #15861, #10570, #4137, #20904, #17884, #3915, #16085, #11016, #19547, #3804, #654, #21126, #5607, #20793, #2446, #15641, #14068, #14400, #17552, #21232, #334, #7090, #17658, #2119, #7202, #5714, #17440, #7532, #8998, #4021, #19436, #438, #12591, #2009, #8891, #7312, #221, #14183, #21020, #10791, #9106, #10897, #17772, #2338, #4679, #2664, #12918, #21788, #6266, #11228, #14950, #18426, #19764, #14831, #4344, #18097, #9548, #6375, #13026, #13247, #4459, #16409, #11122, #6151, #985, #16514, #12813, #19873, #7859, #4573, #9329, #20092, #16189, #9759 ),
 .UNSPECIFIED., .F., .F.,
 ( 4, 2, 2, 2, 2, 2, 2, 2, 2, 2, 2, 2, 2, 2, 2, 2, 2, 2, 2, 2, 2, 2, 2, 2, 2, 2, 2, 2, 2, 2, 2, 2, 2, 2, 2, 2, 2, 2, 2, 2, 2, 2, 2, 2, 2, 2, 2, 2, 2, 2, 2, 2, 2, 2, 2, 2, 2, 2, 2, 2, 2, 2, 2, 2, 2, 2, 2, 2, 2, 2, 2, 2, 2, 2, 2, 2, 2, 2, 2, 2, 2, 2, 2, 2, 2, 2, 2, 2, 2, 2, 2, 2, 2, 2, 2, 2, 2, 2, 2, 2, 2, 2, 2, 2, 2, 2, 2, 2, 2, 2, 2, 2, 2, 2, 2, 2, 2, 2, 2, 2, 2, 2, 2, 2, 2, 2, 2, 2, 2, 2, 2, 2, 2, 2, 2, 2, 2, 2, 2, 2, 2, 2, 2, 2, 2, 2, 2, 2, 2, 2, 2, 2, 2, 2, 2, 2, 2, 2, 2, 2, 2, 2, 2, 4 ),
 ( 0.000000000000000000, 0.001952908952989333875, 0.003905817905978667751, 0.007323408573709997045, 0.01074099924144132634, 0.01415858990917265650, 0.01586738524303832332, 0.01757618057690398666, 0.02099377124463531682, 0.02441136191236664699, 0.02782895258009797368, 0.03124654324782930384, 0.03466413391556063400, 0.03808172458329196070, 0.04149931525102329433, 0.04491690591875462102, 0.04662570125262028436, 0.04833449658648594771, 0.05175208725421727440, 0.05346088258808293775, 0.05516967792194860110, 0.05858726858967993473, 0.06200485925741126836, 0.06542244992514259505, 0.06884004059287393562, 0.07225763126060526231, 0.07567522192833658901, 0.07909281259606792958, 0.08251040326379925627, 0.08421919859766491268, 0.08592799393153058296, 0.08934558459926195129, 0.09276317526699331961, 0.09447197060085900377, 0.09618076593472468794, 0.09959835660245604239, 0.1030159472701873968, 0.1064335379379187652, 0.1098511286056501335, 0.1132687192733815018, 0.1166863099411127869, 0.1201039006088440858, 0.1235214912765753847, 0.1252302866104410273, 0.1269390819443066698, 0.1303566726120379826, 0.1320654679459036251, 0.1337742632797692399, 0.1371918539475005527, 0.1406094446152318378, 0.1440270352829631784, 0.1474446259506944912, 0.1508622166184258040, 0.1542798072861571446, 0.1576973979538884851, 0.1611149886216198257, 0.1645325792893511663, 0.1679501699570824791, 0.1713677606248137919, 0.1747853512925451325, 0.1764941466264108028, 0.1782029419602764730, 0.1816205326280078136, 0.1850381232957391542, 0.1884557139634704670, 0.1918733046312017798, 0.1952908952989331204, 0.1987084859666644887, 0.2021260766343957738, 0.2055436673021270866, 0.2072524626359927569, 0.2089612579698584272, 0.2123788486375897677, 0.2140876439714554380, 0.2157964393053211083, 0.2192140299730524489, 0.2226316206407837617, 0.2260492113085151300, 0.2294668019762464706, 0.2328843926439778111, 0.2363019833117091517, 0.2397195739794404923, 0.2431371646471718329, 0.2465547553149031734, 0.2499723459826345140, 0.2533899366503657991, 0.2568075273180971396, 0.2602251179858284802, 0.2636427086535597653, 0.2670602993212910503, 0.2704778899890223909, 0.2738954806567537315, 0.2773130713244850165, 0.2807306619922163571, 0.2841482526599476977, 0.2858570479938133402, 0.2875658433276790382, 0.2909834339954103788, 0.2926922293292760768, 0.2944010246631417194, 0.2978186153308730599, 0.3012362059986043450, 0.3046537966663356856, 0.3080713873340670261, 0.3114889780017983112, 0.3149065686695296518, 0.3183241593372609368, 0.3217417500049923329, 0.3234505453388579754, 0.3251593406727236735, 0.3285769313404549585, 0.3319945220081862991, 0.3354121126759176397, 0.3388297033436489247, 0.3422472940113802653, 0.3456648846791116059, 0.3490824753468429464, 0.3525000660145742870, 0.3559176566823056276, 0.3593352473500369682, 0.3627528380177683087, 0.3661704286854996493, 0.3695880193532309343, 0.3730056100209622749, 0.3747144053548279174, 0.3764232006886936155, 0.3798407913564249005, 0.3832583820241562411, 0.3866759726918875817, 0.3900935633596189223, 0.3935111540273502628, 0.3969287446950816034, 0.4003463353628129440, 0.4037639260305442845, 0.4054727213644099271, 0.4071815166982756251, 0.4105991073660069102, 0.4140166980337382507, 0.4157254933676038933, 0.4174342887014695913, 0.4208518793692008764, 0.4242694700369322169, 0.4276870607046635575, 0.4311046513723948981, 0.4345222420401262386, 0.4379398327078575237, 0.4413574233755888643, 0.4447750140433202048, 0.4464838093771859029, 0.4481926047110515454, 0.4516101953787828860, 0.4533189907126486395, 0.4550277860465142266, 0.4584453767142455671, 0.4618629673819769077, 0.4652805580497082483, 0.4686981487174395888, 0.4721157393851709294, 0.4755333300529022145, 0.4789509207206335550, 0.4823685113883648956, 0.4840773067222305381, 0.4857861020560962362, 0.4875580825543344710 ),
 .UNSPECIFIED. ) ;
#7347 = CARTESIAN_POINT ( 'NONE',  ( -17.90134810484358141, -14.13951559615540710, -232.9640066987647344 ) ) ;
#7348 = CARTESIAN_POINT ( 'NONE',  ( 1.430961520682887400, 16.89318350835024063, -220.3256763723340157 ) ) ;
#7349 = CARTESIAN_POINT ( 'NONE',  ( -1.177898122437396333, -26.14463525305933445, -216.8677949074964033 ) ) ;
#7350 = CARTESIAN_POINT ( 'NONE',  ( 8.979547488457603421, 23.24376652602565230, -232.6628827740196357 ) ) ;
#7351 = CARTESIAN_POINT ( 'NONE',  ( 7.292867580403318506, -17.79718201325288263, -215.1213547356373397 ) ) ;
#7352 = DIRECTION ( 'NONE',  ( -0.000000000000000000, 0.000000000000000000, -1.000000000000000000 ) ) ;
#7353 = CARTESIAN_POINT ( 'NONE',  ( 30.47710800431509170, 7.409378661937554789, -223.2007768404241688 ) ) ;
#7354 = DIRECTION ( 'NONE',  ( -1.000000000000000000, 0.000000000000000000, 0.000000000000000000 ) ) ;
#7355 = CARTESIAN_POINT ( 'NONE',  ( 13.66858788651615164, -3.112492835348085407, -221.5154270223497690 ) ) ;
#7356 = CARTESIAN_POINT ( 'NONE',  ( 3.325336547283623378, 18.92213121405483633, -219.7480163085221818 ) ) ;
#7357 = CARTESIAN_POINT ( 'NONE',  ( 30.55431851955342282, 7.682798326916945975, -224.9061577511691610 ) ) ;
#7358 = CARTESIAN_POINT ( 'NONE',  ( 16.64225601860865211, 1.926018578292457928, -220.2177910260893725 ) ) ;
#7359 = CARTESIAN_POINT ( 'NONE',  ( -10.41267218490845181, -10.94250683577548244, -225.3448144993165556 ) ) ;
#7360 = CARTESIAN_POINT ( 'NONE',  ( 3.137667653003819446, 15.44806861187908176, -232.6841782316817842 ) ) ;
#7361 = AXIS2_PLACEMENT_3D ( 'NONE', #18768, #11903, #20323 ) ;
#7362 = FACE_OUTER_BOUND ( 'NONE', #5839, .T. ) ;
#7363 = CARTESIAN_POINT ( 'NONE',  ( -7.625346832407194242, -11.41809035428902064, -218.7189489878062716 ) ) ;
#7364 = CARTESIAN_POINT ( 'NONE',  ( -15.51982305277792307, 19.76957551617798359, -231.4018974401358832 ) ) ;
#7365 = CARTESIAN_POINT ( 'NONE',  ( 13.48097272627202159, 8.509510470709432894, -231.5257201610278059 ) ) ;
#7366 = CARTESIAN_POINT ( 'NONE',  ( -13.92941769543345032, 11.48925904027772127, -219.8938199480626281 ) ) ;
#7367 = ADVANCED_FACE ( 'NONE', ( #5643 ), #1666, .T. ) ;
#7368 = CARTESIAN_POINT ( 'NONE',  ( -2.577721557973523314, 25.83760098923793791, -215.4660676095525389 ) ) ;
#7369 = CARTESIAN_POINT ( 'NONE',  ( 25.85597688020959239, 3.954559836939000039, -230.6766427064781624 ) ) ;
#7370 = CARTESIAN_POINT ( 'NONE',  ( 12.24130115618514125, -19.65891960071846967, -230.7381047918825914 ) ) ;
#7371 = ORIENTED_EDGE ( 'NONE', *, *, #14512, .T. ) ;
#7372 = CARTESIAN_POINT ( 'NONE',  ( 16.43596176044053081, -17.06621466254232544, -232.8418678805942648 ) ) ;
#7373 = EDGE_CURVE ( 'NONE', #14290, #19544, #16118, .T. ) ;
#7374 = CARTESIAN_POINT ( 'NONE',  ( -7.058999618647554541, 24.62458660126260312, -219.6630466582859356 ) ) ;
#7375 = CARTESIAN_POINT ( 'NONE',  ( -13.12488928717151637, 0.000000000000000000, -99.99999999999998579 ) ) ;
#7376 = AXIS2_PLACEMENT_3D ( 'NONE', #1518, #20408, #8723 ) ;
#7377 = CARTESIAN_POINT ( 'NONE',  ( 11.33210854356620523, 22.81476816607802149, -217.8536224460118262 ) ) ;
#7378 = CARTESIAN_POINT ( 'NONE',  ( -17.70471257751854921, -0.5540196600081067624, -232.9322037287452360 ) ) ;
#7379 = CARTESIAN_POINT ( 'NONE',  ( -11.39823187951283501, -7.998194509987097689, -226.8062974464413912 ) ) ;
#7380 = CARTESIAN_POINT ( 'NONE',  ( -8.258403559667634397, -29.80786866836635696, -223.3983869762195127 ) ) ;
#7381 = CARTESIAN_POINT ( 'NONE',  ( -3.071946796551161984, 23.17078151772539485, -231.0066194318698933 ) ) ;
#7382 = DIRECTION ( 'NONE',  ( 0.000000000000000000, 0.000000000000000000, -1.000000000000000000 ) ) ;
#7383 = CARTESIAN_POINT ( 'NONE',  ( 18.30590144060498403, 15.06309558287673767, -219.0459394567220102 ) ) ;
#7384 = CARTESIAN_POINT ( 'NONE',  ( -7.913358619554302642, 16.16796202616373890, -233.0981776325470491 ) ) ;
#7385 = CARTESIAN_POINT ( 'NONE',  ( -14.60180519431160917, 24.46340507526420893, -221.8423643191928534 ) ) ;
#7386 = ORIENTED_EDGE ( 'NONE', *, *, #9658, .T. ) ;
#7387 = CARTESIAN_POINT ( 'NONE',  ( 5.803912621764987456, 13.01725692290267844, -221.8367675400179166 ) ) ;
#7388 = CARTESIAN_POINT ( 'NONE',  ( -15.82036597035495795, 4.920771916499852239, -223.0095317795067160 ) ) ;
#7389 = CARTESIAN_POINT ( 'NONE',  ( 18.03440114592047649, 4.755211820135348155, -216.3599228381250157 ) ) ;
#7390 = CARTESIAN_POINT ( 'NONE',  ( 11.72194121175188997, -15.95900783718691507, -217.6519982781775013 ) ) ;
#7391 = DIRECTION ( 'NONE',  ( 1.000000000000000000, 0.000000000000000000, 0.000000000000000000 ) ) ;
#7392 = ORIENTED_EDGE ( 'NONE', *, *, #17196, .F. ) ;
#7393 = CARTESIAN_POINT ( 'NONE',  ( 10.07175337281514871, 14.76776740066196325, -231.7834566702614723 ) ) ;
#7394 = CARTESIAN_POINT ( 'NONE',  ( -13.61368873860109652, -1.873405602088730859, -231.0542245685610112 ) ) ;
#7395 = LINE ( 'NONE', #5683, #5047 ) ;
#7396 = AXIS2_PLACEMENT_3D ( 'NONE', #15532, #3367, #10249 ) ;
#7397 = TOROIDAL_SURFACE ( 'NONE', #9193, 22.63401512838748175, 3.000000000000002665 ) ;
#7398 = CARTESIAN_POINT ( 'NONE',  ( 7.437838793555467731, -20.85539581353325289, -233.9154700400843865 ) ) ;
#7399 =( NAMED_UNIT ( * ) SI_UNIT ( $, .STERADIAN. ) SOLID_ANGLE_UNIT ( ) );
#7400 = CARTESIAN_POINT ( 'NONE',  ( -9.443239614166923701, 9.388015667058336788, -222.3195230688234290 ) ) ;
#7401 = CARTESIAN_POINT ( 'NONE',  ( -11.39536650977235510, 9.246300577217761330, -228.4898727004871546 ) ) ;
#7402 = CARTESIAN_POINT ( 'NONE',  ( -10.51143808951550085, 11.41308718311005066, -231.3573069600382439 ) ) ;
#7403 = CARTESIAN_POINT ( 'NONE',  ( -12.22852564478610482, -7.025360622849957437, -222.3415469712626589 ) ) ;
#7404 = DIRECTION ( 'NONE',  ( 0.000000000000000000, 0.000000000000000000, -1.000000000000000000 ) ) ;
#7405 = CARTESIAN_POINT ( 'NONE',  ( -20.72032262650141021, 9.983465205454267632, 0.6641006075881642490 ) ) ;
#7406 = CARTESIAN_POINT ( 'NONE',  ( -24.68906941503829700, 2.445024713909649705, -232.6803430500543755 ) ) ;
#7407 = CARTESIAN_POINT ( 'NONE',  ( 9.745394341301471641, -28.41975495766811832, -225.7559345954832963 ) ) ;
#7408 = CARTESIAN_POINT ( 'NONE',  ( 14.03916608299427082, 11.26328028684000415, -220.2447382113059007 ) ) ;
#7409 = CARTESIAN_POINT ( 'NONE',  ( -9.503027668167838726, 6.959046566381404730, -225.7241663910276941 ) ) ;
#7410 = CARTESIAN_POINT ( 'NONE',  ( -21.89065952084848021, -0.9940043559354364566, -216.9999999999999716 ) ) ;
#7411 = CARTESIAN_POINT ( 'NONE',  ( 13.72034832542693827, 10.98995328009155692, -220.6189139471235592 ) ) ;
#7412 = CARTESIAN_POINT ( 'NONE',  ( -3.332878961853828592, -21.58676603248690284, -218.0452238110532619 ) ) ;
#7413 = ORIENTED_EDGE ( 'NONE', *, *, #12216, .T. ) ;
#7414 = VECTOR ( 'NONE', #17361, 1000.000000000000000 ) ;
#7415 = CARTESIAN_POINT ( 'NONE',  ( -4.866400999161825780, 25.69921167300892861, -231.0100031340613782 ) ) ;
#7416 = EDGE_CURVE ( 'NONE', #8548, #19867, #4176, .T. ) ;
#7417 = CARTESIAN_POINT ( 'NONE',  ( -13.01542355754912172, 26.77630951171455820, -225.1545229496516356 ) ) ;
#7418 = CARTESIAN_POINT ( 'NONE',  ( -16.40095417437164471, 2.582410108382750646, -233.5151473761628154 ) ) ;
#7419 = CARTESIAN_POINT ( 'NONE',  ( -15.65248652229887405, -15.36320747609890169, -219.0899148657056230 ) ) ;
#7420 = CYLINDRICAL_SURFACE ( 'NONE', #20796, 2.100000000000000089 ) ;
#7421 = ORIENTED_EDGE ( 'NONE', *, *, #8542, .F. ) ;
#7422 = CARTESIAN_POINT ( 'NONE',  ( -22.47200958260654957, 4.697452857301940732, -216.5879371680706242 ) ) ;
#7423 = CARTESIAN_POINT ( 'NONE',  ( 0.6532050297617689738, -21.40793743009686878, -217.7635283671393722 ) ) ;
#7424 = CARTESIAN_POINT ( 'NONE',  ( 17.97843143658897347, 22.12221935793617078, -220.9346589834416079 ) ) ;
#7425 = CARTESIAN_POINT ( 'NONE',  ( 4.603870848087811218, 30.13529352683433515, -225.9623629403671430 ) ) ;
#7426 = UNCERTAINTY_MEASURE_WITH_UNIT (LENGTH_MEASURE( 1.000000000000000082E-05 ), #20271, 'distance_accuracy_value', 'NONE');
#7427 = VECTOR ( 'NONE', #21267, 1000.000000000000000 ) ;
#7428 = CARTESIAN_POINT ( 'NONE',  ( -21.01482965301294925, 6.368220028842532798, -231.7530032521518990 ) ) ;
#7429 = CARTESIAN_POINT ( 'NONE',  ( 2.008896548638861024, 20.64812324442097591, -233.5818019448501843 ) ) ;
#7430 = LINE ( 'NONE', #10692, #2273 ) ;
#7431 = CARTESIAN_POINT ( 'NONE',  ( -6.012234575298915473, -13.00555924700598709, -229.4955436083688483 ) ) ;
#7432 = CARTESIAN_POINT ( 'NONE',  ( 11.90144651507291051, -8.898305237537579515, -228.5592478859710184 ) ) ;
#7433 = DIRECTION ( 'NONE',  ( -1.000000000000000000, 0.000000000000000000, 0.000000000000000000 ) ) ;
#7434 = CYLINDRICAL_SURFACE ( 'NONE', #17339, 23.00000000000000000 ) ;
#7435 = CARTESIAN_POINT ( 'NONE',  ( -10.59650102373989533, 7.849913810122476576, -230.0486530042683171 ) ) ;
#7436 = CARTESIAN_POINT ( 'NONE',  ( -18.47336874364275516, -4.831184938305232990, -219.8627234292127639 ) ) ;
#7437 = CARTESIAN_POINT ( 'NONE',  ( -26.11114532382342901, 12.73400870066318902, -227.7653936945517046 ) ) ;
#7438 = CARTESIAN_POINT ( 'NONE',  ( 20.26651059498356844, 18.95255124124090074, -231.7206897233655525 ) ) ;
#7439 = CARTESIAN_POINT ( 'NONE',  ( 1.313727069624702981, 17.80710275190598324, -219.4197901500037062 ) ) ;
#7440 = ORIENTED_EDGE ( 'NONE', *, *, #473, .F. ) ;
#7441 = CARTESIAN_POINT ( 'NONE',  ( 17.90345650676399814, -22.75668921074696982, -218.1849408917474022 ) ) ;
#7442 = ORIENTED_EDGE ( 'NONE', *, *, #12595, .F. ) ;
#7443 = CARTESIAN_POINT ( 'NONE',  ( 25.33562512631297281, 12.25422971834577268, -228.6777356031426791 ) ) ;
#7444 = CARTESIAN_POINT ( 'NONE',  ( -4.424820997438546399, 11.84746159238278373, -221.7815792475208525 ) ) ;
#7445 = CARTESIAN_POINT ( 'NONE',  ( -5.340143745732740754, 22.10628181454592678, -235.0476201740528097 ) ) ;
#7446 = CARTESIAN_POINT ( 'NONE',  ( -21.27082149447729620, -6.316573346028001801, -216.2864220516500779 ) ) ;
#7447 = CARTESIAN_POINT ( 'NONE',  ( -12.31207293045244988, 6.732038552366256923, -221.0952066824360713 ) ) ;
#7448 = CARTESIAN_POINT ( 'NONE',  ( 4.825543794723634150, -13.95218839875094119, 92.99999999999997158 ) ) ;
#7449 = CARTESIAN_POINT ( 'NONE',  ( 17.43540344723615476, -3.335533435063737340, -230.8961756483947738 ) ) ;
#7450 = CARTESIAN_POINT ( 'NONE',  ( -15.95412330064426065, 13.09400588185824077, -218.6613039563597169 ) ) ;
#7451 = CARTESIAN_POINT ( 'NONE',  ( 18.59615491886314231, -0.2392802120807639710, -217.5848846836084078 ) ) ;
#7452 = CARTESIAN_POINT ( 'NONE',  ( -18.71530386740073126, -0.6857509888707814527, -217.6195632122020527 ) ) ;
#7453 = CARTESIAN_POINT ( 'NONE',  ( 11.87982377808925527, 10.85265283465803421, -229.5027252913499183 ) ) ;
#7454 = CARTESIAN_POINT ( 'NONE',  ( -13.63272521699743756, -3.226083955879493814, -228.1383267723209656 ) ) ;
#7455 = EDGE_LOOP ( 'NONE', ( #14480, #15948, #5925, #2200, #9544 ) ) ;
#7456 = CARTESIAN_POINT ( 'NONE',  ( 2.208705534715813101, 15.26926593729510984, -227.3643075380122980 ) ) ;
#7457 = CARTESIAN_POINT ( 'NONE',  ( -5.279374154171231126, -12.28263746854076466, -222.5283095625445640 ) ) ;
#7458 = CARTESIAN_POINT ( 'NONE',  ( 15.85665641241444668, 18.24713744004561988, -217.7195292979064902 ) ) ;
#7459 = CARTESIAN_POINT ( 'NONE',  ( 3.585135836405817233, -11.76492230538331896, -228.1718440842192024 ) ) ;
#7460 = DIRECTION ( 'NONE',  ( 1.000000000000000000, 0.000000000000000000, 0.000000000000000000 ) ) ;
#7461 = CARTESIAN_POINT ( 'NONE',  ( -12.82737030338386219, 8.595865151885988098, -221.6735325378515142 ) ) ;
#7462 = CARTESIAN_POINT ( 'NONE',  ( 22.46263922039936745, -3.404486942579552089, -216.1438077301478415 ) ) ;
#7463 = CARTESIAN_POINT ( 'NONE',  ( 2.659252340503933443, 26.58135124637517777, -228.4751214701929314 ) ) ;
#7464 = CARTESIAN_POINT ( 'NONE',  ( -13.88743542672353826, 10.36310385030668613, -230.6144170796622745 ) ) ;
#7465 = CARTESIAN_POINT ( 'NONE',  ( 22.03647168420945590, 0.3315607655625663064, -232.0572713672586644 ) ) ;
#7466 = CARTESIAN_POINT ( 'NONE',  ( -7.913663017152074097, -13.07021161337726944, -228.8713148165744258 ) ) ;
#7467 = CARTESIAN_POINT ( 'NONE',  ( 14.96462366732929716, 7.179279272144128754, -233.2042342402542374 ) ) ;
#7468 = PLANE ( 'NONE',  #3351 ) ;
#7469 = CARTESIAN_POINT ( 'NONE',  ( -5.618619326056525587, -15.54696343407853654, -233.4463397655492543 ) ) ;
#7470 = CARTESIAN_POINT ( 'NONE',  ( 2.785859284650920031, 14.19821255961969619, -226.9946081512528906 ) ) ;
#7471 = CARTESIAN_POINT ( 'NONE',  ( 8.903385417657583289, 10.41040586594612272, -227.6527940987422198 ) ) ;
#7472 = CARTESIAN_POINT ( 'NONE',  ( -12.15411956849120756, 11.21601165624538687, -228.1895064089065670 ) ) ;
#7473 = CARTESIAN_POINT ( 'NONE',  ( -0.3984245442872364484, 11.77931270252508789, -223.1826369159892920 ) ) ;
#7474 = CARTESIAN_POINT ( 'NONE',  ( 18.78616100366561881, 3.045752412654093355, -231.5393376370170699 ) ) ;
#7475 = EDGE_CURVE ( 'NONE', #12803, #18886, #16451, .T. ) ;
#7476 = ORIENTED_EDGE ( 'NONE', *, *, #12728, .F. ) ;
#7477 = CARTESIAN_POINT ( 'NONE',  ( 12.70100985296128115, -15.77027744429350165, -219.4156470604730202 ) ) ;
#7478 = ORIENTED_EDGE ( 'NONE', *, *, #21324, .F. ) ;
#7479 = CARTESIAN_POINT ( 'NONE',  ( 10.44758276073090109, -14.65753298717242714, -218.5965683461722904 ) ) ;
#7480 = CARTESIAN_POINT ( 'NONE',  ( -7.770318051073092036, 21.02940971564074957, -231.8751410922876630 ) ) ;
#7481 = ORIENTED_EDGE ( 'NONE', *, *, #6789, .F. ) ;
#7482 = PLANE ( 'NONE',  #4109 ) ;
#7483 = CARTESIAN_POINT ( 'NONE',  ( 14.85123888640019452, 5.067529763532427012, -221.9058491819374979 ) ) ;
#7484 = CARTESIAN_POINT ( 'NONE',  ( 26.48152825632016061, -2.044474411990439666, -219.3412966555575565 ) ) ;
#7485 = CARTESIAN_POINT ( 'NONE',  ( -16.75313578746775889, -14.38352658620038937, -216.6304878158699978 ) ) ;
#7486 = CARTESIAN_POINT ( 'NONE',  ( -2.270280637033633475, -14.48864307936496765, -230.4581659391201072 ) ) ;
#7487 = CARTESIAN_POINT ( 'NONE',  ( 3.281983756374524663, 15.83593597903271721, -223.8697822987047346 ) ) ;
#7488 = CARTESIAN_POINT ( 'NONE',  ( 25.50000000000000000, 0.5000000000000000000, -6.000000000000000000 ) ) ;
#7489 = CARTESIAN_POINT ( 'NONE',  ( -25.59521542166570640, 7.637420400166985424, -216.4190921938142935 ) ) ;
#7490 = CARTESIAN_POINT ( 'NONE',  ( -9.443239614166923701, 9.388015667058336788, -222.3195230688234290 ) ) ;
#7491 = CARTESIAN_POINT ( 'NONE',  ( 4.555016420009541989, 17.65848956729471197, -229.5875910199184204 ) ) ;
#7492 = ORIENTED_EDGE ( 'NONE', *, *, #20798, .F. ) ;
#7493 = CARTESIAN_POINT ( 'NONE',  ( -1.038524475621362075, 14.89017051181998141, -222.3948816610352139 ) ) ;
#7494 = CARTESIAN_POINT ( 'NONE',  ( -11.79656379827575918, 10.43402410864828589, -226.0519616335988076 ) ) ;
#7495 = CARTESIAN_POINT ( 'NONE',  ( 26.56239871811266440, 9.439457669498057868, -217.7226690415261885 ) ) ;
#7496 = EDGE_CURVE ( 'NONE', #14323, #2661, #14623, .T. ) ;
#7497 = CARTESIAN_POINT ( 'NONE',  ( 19.33791609681259160, -22.44220124466257360, -223.0821732511882090 ) ) ;
#7498 = FACE_OUTER_BOUND ( 'NONE', #1703, .T. ) ;
#7499 = ORIENTED_EDGE ( 'NONE', *, *, #19590, .F. ) ;
#7500 = CARTESIAN_POINT ( 'NONE',  ( 11.13678936984666912, 26.95732789089726111, -228.8350761760834757 ) ) ;
#7501 = CARTESIAN_POINT ( 'NONE',  ( -15.42652243319914085, -1.944528292506083167, -233.0911082444762030 ) ) ;
#7502 = DIRECTION ( 'NONE',  ( 0.000000000000000000, 0.000000000000000000, 1.000000000000000000 ) ) ;
#7503 = VECTOR ( 'NONE', #21094, 1000.000000000000000 ) ;
#7504 = CARTESIAN_POINT ( 'NONE',  ( 1.729916699924999746, -18.64927252049523432, -233.5000329212076906 ) ) ;
#7505 = APPLICATION_PROTOCOL_DEFINITION ( 'draft international standard', 'automotive_design', 1998, #19483 ) ;
#7506 = CARTESIAN_POINT ( 'NONE',  ( -9.749377714296398878, 10.28442384816749922, -229.3722863967025205 ) ) ;
#7507 = CARTESIAN_POINT ( 'NONE',  ( -14.30586181932858914, 18.69563132175512266, -215.8217153853723573 ) ) ;
#7508 = ORIENTED_EDGE ( 'NONE', *, *, #20553, .T. ) ;
#7509 = CARTESIAN_POINT ( 'NONE',  ( -10.65455960636934662, 10.37188583052882862, -219.5197110153079620 ) ) ;
#7510 = CARTESIAN_POINT ( 'NONE',  ( -10.71823000853037655, -10.52987076429259794, -221.3501620068516331 ) ) ;
#7511 = DIRECTION ( 'NONE',  ( -1.000000000000000000, 0.000000000000000000, 0.000000000000000000 ) ) ;
#7512 = CARTESIAN_POINT ( 'NONE',  ( -22.62231062914085555, 4.162462751021892338, -9.098484481344788932 ) ) ;
#7513 = CARTESIAN_POINT ( 'NONE',  ( -17.17400284685640344, 24.63223427531467280, -220.6313524368512162 ) ) ;
#7514 = CARTESIAN_POINT ( 'NONE',  ( 8.654719819004025538, -19.13368099829532909, -232.5229659899653711 ) ) ;
#7515 = CARTESIAN_POINT ( 'NONE',  ( -10.65455960636934662, 10.37188583052882862, -219.5197110153079620 ) ) ;
#7516 = CARTESIAN_POINT ( 'NONE',  ( 14.73597170006453361, 7.272367905564328439, -221.0092474305599239 ) ) ;
#7517 = CARTESIAN_POINT ( 'NONE',  ( 2.085064686336211892, 14.99578618537741548, -226.0985834012817861 ) ) ;
#7518 = AXIS2_PLACEMENT_3D ( 'NONE', #2873, #1201, #4238 ) ;
#7519 = CARTESIAN_POINT ( 'NONE',  ( 1.665334536937734811E-13, -24.63401512838747820, -77.51594804401857175 ) ) ;
#7520 = CARTESIAN_POINT ( 'NONE',  ( 17.24423567610276109, 8.542587572837451404, -218.6562240232607621 ) ) ;
#7521 = CARTESIAN_POINT ( 'NONE',  ( -13.89163392164661204, -16.46234366268243221, -230.8566716434345949 ) ) ;
#7522 = ORIENTED_EDGE ( 'NONE', *, *, #11520, .F. ) ;
#7523 = CARTESIAN_POINT ( 'NONE',  ( -3.494873682963683059, 27.70407912598904687, -220.5214894769905243 ) ) ;
#7524 = CARTESIAN_POINT ( 'NONE',  ( -12.15411956849120756, 11.21601165624538687, -228.1895064089065670 ) ) ;
#7525 = CARTESIAN_POINT ( 'NONE',  ( -17.07051451008491938, 15.19890664381897949, -233.6014043774825666 ) ) ;
#7526 = ORIENTED_EDGE ( 'NONE', *, *, #10754, .F. ) ;
#7527 = CARTESIAN_POINT ( 'NONE',  ( -15.15256618962804858, -12.22297499669621423, -230.3735341043967821 ) ) ;
#7528 = DIRECTION ( 'NONE',  ( 0.000000000000000000, 0.000000000000000000, -1.000000000000000000 ) ) ;
#7529 = ORIENTED_EDGE ( 'NONE', *, *, #21928, .T. ) ;
#7530 = CARTESIAN_POINT ( 'NONE',  ( -20.94800339253696109, 4.477632454355491731, -216.5423208360950298 ) ) ;
#7531 = CARTESIAN_POINT ( 'NONE',  ( -0.4195811904800660352, -16.41067541138124852, -229.4634529720845819 ) ) ;
#7532 = CARTESIAN_POINT ( 'NONE',  ( 21.53262694368047647, 11.06794636811408594, -231.8394491640143826 ) ) ;
#7533 = CARTESIAN_POINT ( 'NONE',  ( -3.643097910890548796, 22.16888955197135047, -233.9701981029593298 ) ) ;
#7534 = CARTESIAN_POINT ( 'NONE',  ( -26.70018640714903668, 3.110792036746048428, -228.8761207540193823 ) ) ;
#7535 = CARTESIAN_POINT ( 'NONE',  ( 11.75630001506626776, 9.075791953625659048, -230.4239556728226717 ) ) ;
#7536 = CARTESIAN_POINT ( 'NONE',  ( 14.68783945462866924, 9.535285537539673228, -219.4694094309942045 ) ) ;
#7537 = CARTESIAN_POINT ( 'NONE',  ( 0.000000000000000000, 0.000000000000000000, -105.0000000000000142 ) ) ;
#7538 = CARTESIAN_POINT ( 'NONE',  ( -16.75313578746775889, -14.38352658620038937, -216.6304878158699978 ) ) ;
#7539 = CARTESIAN_POINT ( 'NONE',  ( 2.513843158659109456, -14.78137297724497401, -219.3443999184743518 ) ) ;
#7540 = DIRECTION ( 'NONE',  ( 0.000000000000000000, 0.000000000000000000, 1.000000000000000000 ) ) ;
#7541 = CARTESIAN_POINT ( 'NONE',  ( -12.14471622011552832, 3.716031503296523653, -220.6237729066402835 ) ) ;
#7542 = CARTESIAN_POINT ( 'NONE',  ( 12.49911899277810434, -1.774523103166953497, -229.0731493570444002 ) ) ;
#7543 = CARTESIAN_POINT ( 'NONE',  ( -26.38808873681881906, 13.30696350521622939, -225.1492950792419663 ) ) ;
#7544 = CARTESIAN_POINT ( 'NONE',  ( 6.491278574642851851, 13.23281603069746382, -229.0355254242266767 ) ) ;
#7545 = CARTESIAN_POINT ( 'NONE',  ( 9.280831573919673616, 14.67893982993557422, -228.6940810986570796 ) ) ;
#7546 = EDGE_CURVE ( 'NONE', #16572, #4483, #16413, .T. ) ;
#7547 = ORIENTED_EDGE ( 'NONE', *, *, #21773, .F. ) ;
#7548 = CARTESIAN_POINT ( 'NONE',  ( 12.00030915192824565, -12.23229153226815313, -233.8665814532129730 ) ) ;
#7549 = CARTESIAN_POINT ( 'NONE',  ( 13.69275646168278371, 8.674223198772375909, -220.8699857572541987 ) ) ;
#7550 = CARTESIAN_POINT ( 'NONE',  ( -5.028549462823471039, 18.55099042571767143, -234.6264744246184648 ) ) ;
#7551 = CARTESIAN_POINT ( 'NONE',  ( -4.619644865335168049, 14.75104250038670450, -232.3086264397671812 ) ) ;
#7552 = CARTESIAN_POINT ( 'NONE',  ( -28.74911369566071784, -10.37195270599671737, -225.4617258471509729 ) ) ;
#7553 = CARTESIAN_POINT ( 'NONE',  ( -11.24282496690421596, 12.44430180464951086, -232.4405891940542404 ) ) ;
#7554 = CARTESIAN_POINT ( 'NONE',  ( -13.95218839875094119, -4.825543794723769153, 93.00000000000000000 ) ) ;
#7555 = CARTESIAN_POINT ( 'NONE',  ( 15.05575868828727515, -2.428864548505686560, -227.9368649688638584 ) ) ;
#7556 = CARTESIAN_POINT ( 'NONE',  ( -5.562203253303141359, 12.75725363875033302, -225.3078268727488478 ) ) ;
#7557 = CARTESIAN_POINT ( 'NONE',  ( 29.00474534066713872, 11.29707752057770698, -221.8682176444242771 ) ) ;
#7558 = CARTESIAN_POINT ( 'NONE',  ( -22.17339560624464312, 16.26550580028390769, -232.0582861498566274 ) ) ;
#7559 = CARTESIAN_POINT ( 'NONE',  ( 9.586902571418640662, 24.43292817174309661, -231.9968623198229807 ) ) ;
#7560 = CARTESIAN_POINT ( 'NONE',  ( -24.63401512838748530, 3.016796777712720900E-15, -77.51594804401857175 ) ) ;
#7561 = ORIENTED_EDGE ( 'NONE', *, *, #10221, .F. ) ;
#7562 = CARTESIAN_POINT ( 'NONE',  ( 4.238595127209166868, 26.19205419861516404, -230.1142052665570077 ) ) ;
#7563 = CARTESIAN_POINT ( 'NONE',  ( -11.36971918743327237, -8.287084598727400220, -223.1364763414170227 ) ) ;
#7564 = CARTESIAN_POINT ( 'NONE',  ( 3.449504654906655254, 27.59247159270940841, -231.3461799890608859 ) ) ;
#7565 = CARTESIAN_POINT ( 'NONE',  ( 13.17462184258262070, -16.01403271225657932, -214.6792330615317610 ) ) ;
#7566 = CARTESIAN_POINT ( 'NONE',  ( 0.000000000000000000, 0.000000000000000000, -77.51594804401857175 ) ) ;
#7567 = EDGE_CURVE ( 'NONE', #7956, #5604, #15692, .T. ) ;
#7568 = CARTESIAN_POINT ( 'NONE',  ( -11.48592899399814726, 13.65854631785387774, -230.8311022452805616 ) ) ;
#7569 = CARTESIAN_POINT ( 'NONE',  ( 0.000000000000000000, 0.000000000000000000, -55.00000000000000711 ) ) ;
#7570 = CARTESIAN_POINT ( 'NONE',  ( 16.18295504345472580, -4.390854861972272261, -232.0514848646187716 ) ) ;
#7571 = CARTESIAN_POINT ( 'NONE',  ( 1.820119372073704112, 23.17972341190215246, -230.7270437017659503 ) ) ;
#7572 = CARTESIAN_POINT ( 'NONE',  ( -12.06153928353927540, 8.661506524875534296, -226.8425068572842349 ) ) ;
#7573 = CARTESIAN_POINT ( 'NONE',  ( 14.63113973005795643, 4.926264598692385199, -222.4866305912601945 ) ) ;
#7574 = CARTESIAN_POINT ( 'NONE',  ( -15.71547198132422984, -24.70787285779005060, -226.7356521228395536 ) ) ;
#7575 = CARTESIAN_POINT ( 'NONE',  ( 10.00603923119254723, 9.610873433734882454, -231.2388095806506669 ) ) ;
#7576 = CARTESIAN_POINT ( 'NONE',  ( 0.000000000000000000, 21.00000000000000000, 75.00000000000000000 ) ) ;
#7577 = CARTESIAN_POINT ( 'NONE',  ( -21.38010734112553024, -21.14131910627544997, -218.4623475309535365 ) ) ;
#7578 = CARTESIAN_POINT ( 'NONE',  ( 8.860681144154234801, 27.11956268701432293, -229.8503778060109823 ) ) ;
#7579 = CARTESIAN_POINT ( 'NONE',  ( 15.91624278015930649, 5.932232821383347954, -217.3600859879243217 ) ) ;
#7580 = CARTESIAN_POINT ( 'NONE',  ( -18.36252859017411510, 21.06344830687906367, -228.5073589488702623 ) ) ;
#7581 = CARTESIAN_POINT ( 'NONE',  ( -2.218529449563984901, 24.06491599887877442, -214.8915873797660652 ) ) ;
#7582 = CARTESIAN_POINT ( 'NONE',  ( -21.08008464085897060, -0.9048411197481797119, -217.0000000010748522 ) ) ;
#7583 = CARTESIAN_POINT ( 'NONE',  ( 2.864019721262919926, -25.46936398327173379, -230.7696170053991978 ) ) ;
#7584 = EDGE_LOOP ( 'NONE', ( #10743, #12204, #17649, #3982 ) ) ;
#7585 = CARTESIAN_POINT ( 'NONE',  ( 18.03651828442428595, -19.10816016050398147, -231.7458924702002037 ) ) ;
#7586 = CARTESIAN_POINT ( 'NONE',  ( 17.99029889091409018, 9.613712288440757092, -232.0298403238024036 ) ) ;
#7587 = CARTESIAN_POINT ( 'NONE',  ( -28.96081738894762125, -0.4213479615504204800, -230.3891733152809707 ) ) ;
#7588 = CARTESIAN_POINT ( 'NONE',  ( -14.40111287326894640, -6.123720356435734757, -220.5571602876142094 ) ) ;
#7589 = CARTESIAN_POINT ( 'NONE',  ( -9.606889355748592152, -11.26588727105406385, -229.9123324032181586 ) ) ;
#7590 = CARTESIAN_POINT ( 'NONE',  ( 7.487569386194327770, 15.49107591903592862, -229.0624668269501001 ) ) ;
#7591 = DIRECTION ( 'NONE',  ( 0.000000000000000000, 0.000000000000000000, -1.000000000000000000 ) ) ;
#7592 = CARTESIAN_POINT ( 'NONE',  ( 14.02802030611117878, 3.063901161068346646, -225.6350222114233475 ) ) ;
#7593 = CARTESIAN_POINT ( 'NONE',  ( -2.698926868850080041, 12.89339462271858316, -226.7595176699009585 ) ) ;
#7594 = CARTESIAN_POINT ( 'NONE',  ( 3.673290835002071653, 15.92545533070904895, -226.4848186297188022 ) ) ;
#7595 = CARTESIAN_POINT ( 'NONE',  ( 12.37876697492742650, -4.127359938151530905, -227.8507160500782618 ) ) ;
#7596 = VERTEX_POINT ( 'NONE', #17811 ) ;
#7597 = ORIENTED_EDGE ( 'NONE', *, *, #21161, .F. ) ;
#7598 = CARTESIAN_POINT ( 'NONE',  ( 21.26803326031697949, 19.54255073453192892, -230.5813148908474659 ) ) ;
#7599 = CARTESIAN_POINT ( 'NONE',  ( -22.19349712985372491, 11.03542788991621748, -219.7744882786627443 ) ) ;
#7600 = CARTESIAN_POINT ( 'NONE',  ( 20.09685469220202236, -2.033783885649083079, -233.1448060988079760 ) ) ;
#7601 = CARTESIAN_POINT ( 'NONE',  ( -4.994543945659216000, -15.01629888130124435, -221.3392717856295633 ) ) ;
#7602 = DIRECTION ( 'NONE',  ( 0.000000000000000000, 0.000000000000000000, 1.000000000000000000 ) ) ;
#7603 = CARTESIAN_POINT ( 'NONE',  ( -21.63401512838757768, 2.649402737968526106E-15, 77.51594804401857175 ) ) ;
#7604 = EDGE_CURVE ( 'NONE', #21555, #14126, #16336, .T. ) ;
#7605 = CARTESIAN_POINT ( 'NONE',  ( 4.484811161826725900, 15.38298568785217313, -219.4617573400562662 ) ) ;
#7606 = CARTESIAN_POINT ( 'NONE',  ( 20.29112488791128399, -13.23242053965672049, -219.3899762660180102 ) ) ;
#7607 = FACE_BOUND ( 'NONE', #14199, .T. ) ;
#7608 = CARTESIAN_POINT ( 'NONE',  ( -8.257247207528708444, -26.39349301559143512, -217.9383130379005138 ) ) ;
#7609 = APPLICATION_PROTOCOL_DEFINITION ( 'draft international standard', 'automotive_design', 1998, #8297 ) ;
#7610 = CARTESIAN_POINT ( 'NONE',  ( 5.331555957413248059, 27.50712867803999728, -219.0801070358024276 ) ) ;
#7611 = CARTESIAN_POINT ( 'NONE',  ( 4.914880347045685660, 14.54749271951947698, -232.8668677254037789 ) ) ;
#7612 = ORIENTED_EDGE ( 'NONE', *, *, #3358, .T. ) ;
#7613 = CARTESIAN_POINT ( 'NONE',  ( -14.73016414256368911, 22.23431809695627237, -217.1425123644553707 ) ) ;
#7614 = CARTESIAN_POINT ( 'NONE',  ( -12.79488508867961549, -11.10380203712096581, -230.9440799972209106 ) ) ;
#7615 = CARTESIAN_POINT ( 'NONE',  ( -25.00000000000013500, 1.972152263052529514E-28, -10.00000000000000000 ) ) ;
#7616 = CARTESIAN_POINT ( 'NONE',  ( -20.71218630467650357, 10.00026692487615065, -0.6553852958034992460 ) ) ;
#7617 = CARTESIAN_POINT ( 'NONE',  ( -2.958555384449997661, 13.07587799061801093, -222.7767538261418565 ) ) ;
#7618 = CARTESIAN_POINT ( 'NONE',  ( 8.222674095483935020, -17.25680718911290512, -231.8150392270642612 ) ) ;
#7619 =( LENGTH_UNIT ( ) NAMED_UNIT ( * ) SI_UNIT ( .MILLI., .METRE. ) );
#7620 = CARTESIAN_POINT ( 'NONE',  ( -9.171998067665157350, 9.395241133357435714, -226.3428046914542051 ) ) ;
#7621 = AXIS2_PLACEMENT_3D ( 'NONE', #3325, #15284, #11668 ) ;
#7622 = CARTESIAN_POINT ( 'NONE',  ( -20.76981451797363576, 10.27702766794165257, -234.3988437453480742 ) ) ;
#7623 = CARTESIAN_POINT ( 'NONE',  ( 1.847452069095833593, 15.11597492720254543, -223.6261404253179421 ) ) ;
#7624 = CARTESIAN_POINT ( 'NONE',  ( 0.000000000000000000, -23.00000000000006040, 75.00000000000000000 ) ) ;
#7625 = CARTESIAN_POINT ( 'NONE',  ( -22.10934047915441170, 0.9940043559354162506, -215.0000000000000000 ) ) ;
#7626 = CARTESIAN_POINT ( 'NONE',  ( -10.71434429704389046, -13.39337408441371124, -228.3296939239235428 ) ) ;
#7627 = ORIENTED_EDGE ( 'NONE', *, *, #17083, .T. ) ;
#7628 = CARTESIAN_POINT ( 'NONE',  ( 11.98894270675143225, 20.38243841428667835, -233.2283128908360084 ) ) ;
#7629 = CARTESIAN_POINT ( 'NONE',  ( -15.15469129103955304, 15.56563882170958024, -231.6314069158229643 ) ) ;
#7630 = CARTESIAN_POINT ( 'NONE',  ( -13.30451247859013897, 19.85560227862636040, -232.3493821534129609 ) ) ;
#7631 = VECTOR ( 'NONE', #10595, 1000.000000000000000 ) ;
#7632 = CARTESIAN_POINT ( 'NONE',  ( -19.35484598183500538, -9.368503549647014594, -231.4111816933332477 ) ) ;
#7633 = FACE_OUTER_BOUND ( 'NONE', #16504, .T. ) ;
#7634 = EDGE_LOOP ( 'NONE', ( #10379, #8677, #102, #18423 ) ) ;
#7635 = CARTESIAN_POINT ( 'NONE',  ( -21.93900267957129557, 7.862893636934532360, -233.4951761057262161 ) ) ;
#7636 = CARTESIAN_POINT ( 'NONE',  ( 5.786710755275625395, -21.74573425722988063, -218.5323380358915131 ) ) ;
#7637 = DIRECTION ( 'NONE',  ( 0.000000000000000000, 0.000000000000000000, 1.000000000000000000 ) ) ;
#7638 = CARTESIAN_POINT ( 'NONE',  ( 4.301648988406530094, 13.23079486486395240, -223.2766268961034655 ) ) ;
#7639 = CARTESIAN_POINT ( 'NONE',  ( 0.000000000000000000, 0.000000000000000000, -55.00000000000000000 ) ) ;
#7640 = CARTESIAN_POINT ( 'NONE',  ( 17.72360441613731652, -1.822637811265336749, -232.2813868768326984 ) ) ;
#7641 = CARTESIAN_POINT ( 'NONE',  ( 12.90536070039565963, 17.66816134723717724, -234.8562535614228750 ) ) ;
#7642 = AXIS2_PLACEMENT_3D ( 'NONE', #7894, #11483, #4275 ) ;
#7643 = EDGE_CURVE ( 'NONE', #2355, #18247, #5976, .T. ) ;
#7644 = CARTESIAN_POINT ( 'NONE',  ( 22.66390650824515873, 11.48342577402021725, -231.3155567808436217 ) ) ;
#7645 = CARTESIAN_POINT ( 'NONE',  ( 18.00000000000000000, 1.360023205165816762E-13, 10.00000000000000000 ) ) ;
#7646 = CARTESIAN_POINT ( 'NONE',  ( -12.28596215050325924, -1.831058988293407852, -228.6496409048244516 ) ) ;
#7647 = CARTESIAN_POINT ( 'NONE',  ( -12.11864581566431553, -23.10742878804749978, -232.9192999331436909 ) ) ;
#7648 = CARTESIAN_POINT ( 'NONE',  ( 1.541778504653760429, -23.48174737203985529, -233.9922866444541967 ) ) ;
#7649 = CARTESIAN_POINT ( 'NONE',  ( -22.77193774148174654, -3.246634745707170033, -9.464084820472235648 ) ) ;
#7650 = CARTESIAN_POINT ( 'NONE',  ( 1.455845656607146304E-13, -21.63401512838760610, 77.51594804401857175 ) ) ;
#7651 = CARTESIAN_POINT ( 'NONE',  ( -1.973648319964989462, 15.33498294326524203, -220.9958390492969329 ) ) ;
#7652 = CARTESIAN_POINT ( 'NONE',  ( 25.75143957690053753, -9.476334075918805055, -216.1442976756887617 ) ) ;
#7653 = CARTESIAN_POINT ( 'NONE',  ( 17.01060404384151781, -6.151862203644831162, -218.3248062500343849 ) ) ;
#7654 = CARTESIAN_POINT ( 'NONE',  ( -14.24491355791863612, 5.286533920242113105, -221.7104936369346433 ) ) ;
#7655 = CARTESIAN_POINT ( 'NONE',  ( 10.88376588832297287, 7.577514201227793400, -222.7215714477710833 ) ) ;
#7656 = CARTESIAN_POINT ( 'NONE',  ( 20.58393751692968721, 18.55948753678544705, -226.8933397075267635 ) ) ;
#7657 = ORIENTED_EDGE ( 'NONE', *, *, #357, .T. ) ;
#7658 = CARTESIAN_POINT ( 'NONE',  ( 12.44757525125794118, -27.84495572490402182, -221.5053358145852656 ) ) ;
#7659 = CARTESIAN_POINT ( 'NONE',  ( 0.000000000000000000, 0.000000000000000000, -78.50000000000000000 ) ) ;
#7660 = AXIS2_PLACEMENT_3D ( 'NONE', #5922, #19322, #17760 ) ;
#7661 = VECTOR ( 'NONE', #14357, 1000.000000000000000 ) ;
#7662 = CARTESIAN_POINT ( 'NONE',  ( -0.2269548806647709305, 12.31484924552052718, -228.6688778050056783 ) ) ;
#7663 = CARTESIAN_POINT ( 'NONE',  ( -4.695076324262313250, 31.85502299853856201, -223.8918597786031341 ) ) ;
#7664 = CARTESIAN_POINT ( 'NONE',  ( -21.14773328851117995, -13.15959238732831693, -217.2646803791660943 ) ) ;
#7665 = CARTESIAN_POINT ( 'NONE',  ( -24.48580119005125866, 9.312492396273500006, -232.5498413856076070 ) ) ;
#7666 = CARTESIAN_POINT ( 'NONE',  ( 21.80000000000000071, 0.000000000000000000, -78.50000000000000000 ) ) ;
#7667 = CARTESIAN_POINT ( 'NONE',  ( 23.12216041205843453, 0.2121350054995089496, -232.0572713672589202 ) ) ;
#7668 = CARTESIAN_POINT ( 'NONE',  ( -8.316505849089994129, 18.84563905716333210, -217.0138378867507640 ) ) ;
#7669 = CARTESIAN_POINT ( 'NONE',  ( 30.65249971456167799, 3.724008896938769464, -225.4815109119605552 ) ) ;
#7670 = CARTESIAN_POINT ( 'NONE',  ( -20.18153419852512442, 14.25141268122526483, -233.5059133483111964 ) ) ;
#7671 = CARTESIAN_POINT ( 'NONE',  ( 23.49048926389013658, 9.645778135078892035, -218.7307869890797463 ) ) ;
#7672 = TOROIDAL_SURFACE ( 'NONE', #10544, 22.63401512838748175, 3.000000000000002665 ) ;
#7673 = AXIS2_PLACEMENT_3D ( 'NONE', #9084, #3999, #7291 ) ;
#7674 = FACE_OUTER_BOUND ( 'NONE', #6880, .T. ) ;
#7675 = CARTESIAN_POINT ( 'NONE',  ( 5.711092584709906106, 26.13380667269736790, -220.5232813324456629 ) ) ;
#7676 = CARTESIAN_POINT ( 'NONE',  ( -20.83683780809167629, -19.66850649927503625, -219.7460615899071570 ) ) ;
#7677 = CARTESIAN_POINT ( 'NONE',  ( 12.99034161053428349, 11.71468708507361889, -230.9043293568357740 ) ) ;
#7678 = CARTESIAN_POINT ( 'NONE',  ( -7.384981288797311194, -12.33405319921006615, -226.2189290763054998 ) ) ;
#7679 = CARTESIAN_POINT ( 'NONE',  ( 18.83061188870378544, 2.941116900365108311, -224.3968446651786337 ) ) ;
#7680 = CARTESIAN_POINT ( 'NONE',  ( -15.11329978779464689, 11.41628732213579411, -231.7124318929555500 ) ) ;
#7681 = SURFACE_STYLE_USAGE ( .BOTH. , #9807 ) ;
#7682 = CARTESIAN_POINT ( 'NONE',  ( -27.13703770709692265, -3.029478475984613173, -219.1636194202163779 ) ) ;
#7683 = CARTESIAN_POINT ( 'NONE',  ( 7.487569386194327770, 15.49107591903592862, -229.0624668269501001 ) ) ;
#7684 = CARTESIAN_POINT ( 'NONE',  ( -25.64868633208605786, 12.30364128039660798, -229.0020209687957049 ) ) ;
#7685 = CARTESIAN_POINT ( 'NONE',  ( -9.924247690135956645, 7.079756654796299564, -222.1205998075789694 ) ) ;
#7686 = CARTESIAN_POINT ( 'NONE',  ( -14.93311267495276518, -24.05029333330348251, -229.1587772033057888 ) ) ;
#7687 = CARTESIAN_POINT ( 'NONE',  ( 29.00474534066713872, 11.29707752057770698, -221.8682176444242771 ) ) ;
#7688 = CIRCLE ( 'NONE', #4072, 2.999999999999999112 ) ;
#7689 = CIRCLE ( 'NONE', #20238, 21.63401512838748175 ) ;
#7690 = CYLINDRICAL_SURFACE ( 'NONE', #812, 23.00000000000008882 ) ;
#7691 = CARTESIAN_POINT ( 'NONE',  ( -9.664312646807834639, -7.057764824546099547, -227.2890491868971594 ) ) ;
#7692 = CARTESIAN_POINT ( 'NONE',  ( -3.494873682963683059, 27.70407912598904687, -220.5214894769905243 ) ) ;
#7693 = CARTESIAN_POINT ( 'NONE',  ( 27.13894094332088969, 12.30518789341946295, -220.2765066586875093 ) ) ;
#7694 = CARTESIAN_POINT ( 'NONE',  ( -11.10144104376680652, 18.49675466419975578, -232.2931259015917647 ) ) ;
#7695 = CARTESIAN_POINT ( 'NONE',  ( 8.454338299486085617, 13.28844197278511530, -217.6979371188311632 ) ) ;
#7696 = CARTESIAN_POINT ( 'NONE',  ( 6.477082923917054202, -23.79794467951758108, -219.1375485160026813 ) ) ;
#7697 = EDGE_LOOP ( 'NONE', ( #14595, #15005, #8240, #5447 ) ) ;
#7698 = CARTESIAN_POINT ( 'NONE',  ( -4.650330424930598561, -23.85841421069521928, -231.7493909980149454 ) ) ;
#7699 = CARTESIAN_POINT ( 'NONE',  ( 28.02123297569005089, 5.903198806000402143, -227.5759114383273811 ) ) ;
#7700 = CARTESIAN_POINT ( 'NONE',  ( 18.00123703865980218, -15.82960056198189491, -233.0014896689109776 ) ) ;
#7701 = CARTESIAN_POINT ( 'NONE',  ( 19.91550388961935525, -0.5333217442993671842, -216.6463151812154138 ) ) ;
#7702 = CARTESIAN_POINT ( 'NONE',  ( -11.06377138986482933, -15.30386857868810857, -217.0411070525910873 ) ) ;
#7703 = CARTESIAN_POINT ( 'NONE',  ( 13.50603691942335693, 22.79443449215731832, -229.7689193854997995 ) ) ;
#7704 = CARTESIAN_POINT ( 'NONE',  ( -2.100000000000000089, 2.571758278209441957E-16, -75.00000000000000000 ) ) ;
#7705 = CARTESIAN_POINT ( 'NONE',  ( -14.83095329101371540, 1.580869236763225549, -217.8331819987577660 ) ) ;
#7706 = CIRCLE ( 'NONE', #20618, 23.00000000000008882 ) ;
#7707 = CARTESIAN_POINT ( 'NONE',  ( 2.837900457371055563, 25.11342719071438978, -232.9871906064174709 ) ) ;
#7708 = CARTESIAN_POINT ( 'NONE',  ( -2.906906946766868227, 27.66682465340607422, -226.6559963821499082 ) ) ;
#7709 = CARTESIAN_POINT ( 'NONE',  ( 17.88855223994683286, -5.550763357372503037, -216.0002797835408614 ) ) ;
#7710 = ORIENTED_EDGE ( 'NONE', *, *, #11000, .F. ) ;
#7711 = CARTESIAN_POINT ( 'NONE',  ( 16.69977105456987232, 16.51652889326612694, -233.6667933521891030 ) ) ;
#7712 = CARTESIAN_POINT ( 'NONE',  ( -18.92390258637512090, 12.75887082072172163, -230.9970325548277970 ) ) ;
#7713 = CARTESIAN_POINT ( 'NONE',  ( -26.91858181626453472, 10.72837452931393187, -223.4556356000267670 ) ) ;
#7714 = CARTESIAN_POINT ( 'NONE',  ( -4.879290506874147226, -14.18937706998098136, -223.0759034783553147 ) ) ;
#7715 = DIRECTION ( 'NONE',  ( 1.000000000000000000, 0.000000000000000000, 0.000000000000000000 ) ) ;
#7716 = ORIENTED_EDGE ( 'NONE', *, *, #10506, .T. ) ;
#7717 = CARTESIAN_POINT ( 'NONE',  ( 5.141746912158045468, 22.01688500372448232, -216.6678693612369386 ) ) ;
#7718 = CARTESIAN_POINT ( 'NONE',  ( 17.16551562789753049, -17.52877442517796780, -218.8649675774640286 ) ) ;
#7719 = CARTESIAN_POINT ( 'NONE',  ( -13.81390866287826746, 1.832988708064121175, -224.4361041349432639 ) ) ;
#7720 = CARTESIAN_POINT ( 'NONE',  ( -12.11864581566431553, -23.10742878804749978, -232.9192999331436909 ) ) ;
#7721 = CARTESIAN_POINT ( 'NONE',  ( 0.4042326456706432647, 15.50845657815858303, -219.2680337625893401 ) ) ;
#7722 = TOROIDAL_SURFACE ( 'NONE', #20274, 22.63401512838748175, 3.000000000000002665 ) ;
#7723 = CARTESIAN_POINT ( 'NONE',  ( -5.191169535941942748, 31.49570301054888688, -227.4714364261087098 ) ) ;
#7724 = ORIENTED_EDGE ( 'NONE', *, *, #21351, .T. ) ;
#7725 = CARTESIAN_POINT ( 'NONE',  ( -11.79584727357715934, 6.509288465425584036, -222.6080315736180921 ) ) ;
#7726 = CARTESIAN_POINT ( 'NONE',  ( 19.99722954683925025, -4.901308424099491745, -217.6076555004800070 ) ) ;
#7727 = CARTESIAN_POINT ( 'NONE',  ( -24.79573179333883814, -3.246809539008099765, 9.480629939678795637 ) ) ;
#7728 = DIRECTION ( 'NONE',  ( -0.000000000000000000, -0.000000000000000000, -1.000000000000000000 ) ) ;
#7729 = CARTESIAN_POINT ( 'NONE',  ( -15.58461825850822180, 18.91734573546571951, -233.7691177939990723 ) ) ;
#7730 = CARTESIAN_POINT ( 'NONE',  ( -5.618619326056525587, -15.54696343407853654, -233.4463397655492543 ) ) ;
#7732 = EDGE_CURVE ( 'NONE', #237, #930, #22164, .T. ) ;
#7731 = CARTESIAN_POINT ( 'NONE',  ( 14.31589812732703670, -5.349901619299376243, -221.2752230612865105 ) ) ;
#7733 = CARTESIAN_POINT ( 'NONE',  ( -17.75316132689678383, 25.03468689048078843, -222.1645193425721061 ) ) ;
#7734 = CARTESIAN_POINT ( 'NONE',  ( -21.07387565400155438, 1.107905485989369554, -215.0000000023499069 ) ) ;
#7735 = CARTESIAN_POINT ( 'NONE',  ( -1.316322971969275502, 14.13179993441458215, -224.9782367179667233 ) ) ;
#7736 = CARTESIAN_POINT ( 'NONE',  ( 0.000000000000000000, 17.50000000000000711, -24.99999999999999645 ) ) ;
#7737 = CARTESIAN_POINT ( 'NONE',  ( -14.83095329101371540, 1.580869236763225549, -217.8331819987577660 ) ) ;
#7738 = CARTESIAN_POINT ( 'NONE',  ( -13.83311471749147259, -24.17028674860418747, -226.2550113133487173 ) ) ;
#7739 = ORIENTED_EDGE ( 'NONE', *, *, #20425, .F. ) ;
#7740 = CARTESIAN_POINT ( 'NONE',  ( 10.03842945413050458, 28.43460431997513638, -225.8374938385031214 ) ) ;
#7741 = CARTESIAN_POINT ( 'NONE',  ( -13.23768812067001477, 12.78288831771969569, -230.4179793829127902 ) ) ;
#7742 = CARTESIAN_POINT ( 'NONE',  ( -21.95649697515285581, 20.70968357470995258, -226.9638023349746447 ) ) ;
#7743 = CARTESIAN_POINT ( 'NONE',  ( -24.66391263913385856, -10.62169550967977472, -229.5175364317193498 ) ) ;
#7744 = DIRECTION ( 'NONE',  ( -1.000000000000000000, 0.000000000000000000, 0.000000000000000000 ) ) ;
#7745 = AXIS2_PLACEMENT_3D ( 'NONE', #18581, #6759, #15209 ) ;
#7746 = ORIENTED_EDGE ( 'NONE', *, *, #6499, .F. ) ;
#7747 = STYLED_ITEM ( 'NONE', ( #1430 ), #13667 ) ;
#7748 = CARTESIAN_POINT ( 'NONE',  ( -29.30406754532526037, 5.063969254119831120, -221.8212091093853076 ) ) ;
#7749 = CARTESIAN_POINT ( 'NONE',  ( -7.253640667752737414, -12.78251829042625687, -230.3353663933772282 ) ) ;
#7750 = CARTESIAN_POINT ( 'NONE',  ( 13.46986076300967028, 0.6273780802722437322, -227.9371333673601043 ) ) ;
#7751 = CARTESIAN_POINT ( 'NONE',  ( -0.1571923090946999446, 19.34188126963334398, -216.6893131123363787 ) ) ;
#7752 = DIRECTION ( 'NONE',  ( 0.000000000000000000, 0.000000000000000000, -1.000000000000000000 ) ) ;
#7753 = CARTESIAN_POINT ( 'NONE',  ( -18.88344489807484905, 1.071113352238720617, -230.0966926586188208 ) ) ;
#7754 = CARTESIAN_POINT ( 'NONE',  ( 12.92410717862594893, 29.37236178718849189, -224.5435071569520744 ) ) ;
#7755 = CARTESIAN_POINT ( 'NONE',  ( 19.19288224840068935, 10.13059690604263174, -232.1906135022504998 ) ) ;
#7756 = CARTESIAN_POINT ( 'NONE',  ( -22.63401512838748175, 0.000000000000000000, -77.51594804401857175 ) ) ;
#7757 = CARTESIAN_POINT ( 'NONE',  ( -14.03169683822311420, -2.573853926495621725, -218.3324423281324016 ) ) ;
#7759 = ADVANCED_FACE ( 'NONE', ( #2593 ), #7901, .F. ) ;
#7758 = CARTESIAN_POINT ( 'NONE',  ( -19.88402822078561627, -6.951120502836210413, -232.7962440186676361 ) ) ;
#7760 = VECTOR ( 'NONE', #16473, 1000.000000000000000 ) ;
#7761 = FACE_OUTER_BOUND ( 'NONE', #8438, .T. ) ;
#7762 = CARTESIAN_POINT ( 'NONE',  ( 0.000000000000000000, 0.000000000000000000, -55.00000000000000000 ) ) ;
#7763 = CARTESIAN_POINT ( 'NONE',  ( -2.125813515909480866, 15.68152656492264363, -220.3943115937447317 ) ) ;
#7764 = CARTESIAN_POINT ( 'NONE',  ( 31.90367160121947876, -0.9372977198352894224, -223.6547426844143445 ) ) ;
#7765 = CARTESIAN_POINT ( 'NONE',  ( 27.92729748684602598, -8.572309054117944527, -222.6487661343338686 ) ) ;
#7766 = CARTESIAN_POINT ( 'NONE',  ( -28.61025869263052712, 6.891613135096296361, -222.2489362813765013 ) ) ;
#7767 = CARTESIAN_POINT ( 'NONE',  ( 9.774133712851615030, 11.09751083462123766, -229.6876724410067823 ) ) ;
#7768 = CARTESIAN_POINT ( 'NONE',  ( 16.29563576379945999, 21.41235115595959826, -221.8114656550040991 ) ) ;
#7769 = ORIENTED_EDGE ( 'NONE', *, *, #3303, .T. ) ;
#7770 = CARTESIAN_POINT ( 'NONE',  ( 3.924989892941122438, -14.79802789183876044, -219.9433972157300445 ) ) ;
#7771 = CARTESIAN_POINT ( 'NONE',  ( -9.946257437971052440, 10.55583158923998077, 93.00000000000001421 ) ) ;
#7772 = ADVANCED_BREP_SHAPE_REPRESENTATION ( '', ( #14254, #6677 ), #8503 ) ;
#7773 = CARTESIAN_POINT ( 'NONE',  ( 4.569118550756183339, 31.72363458735121000, -222.3920438419263519 ) ) ;
#7774 = CARTESIAN_POINT ( 'NONE',  ( -3.687581766460184429, 30.01855770642711718, -218.8323691868875187 ) ) ;
#7775 = CARTESIAN_POINT ( 'NONE',  ( 13.96414008557630559, -4.972932825000588863, -226.4793371398648389 ) ) ;
#7776 = EDGE_CURVE ( 'NONE', #3572, #5555, #19145, .T. ) ;
#7777 = CARTESIAN_POINT ( 'NONE',  ( -3.843007962268670585, 27.94983497691806917, -231.4302614368887703 ) ) ;
#7778 = DIRECTION ( 'NONE',  ( 1.000000000000000000, 0.000000000000000000, -0.000000000000000000 ) ) ;
#7779 = AXIS2_PLACEMENT_3D ( 'NONE', #1991, #12356, #5802 ) ;
#7780 = CIRCLE ( 'NONE', #16377, 22.91388766833460977 ) ;
#7781 = EDGE_CURVE ( 'NONE', #2661, #14323, #7792, .T. ) ;
#7782 = CARTESIAN_POINT ( 'NONE',  ( 1.660345614755502686, 12.19060476922103931, -223.1112690039082906 ) ) ;
#7783 = CARTESIAN_POINT ( 'NONE',  ( 21.06229272850552547, 3.434461253538921621, -234.1452885155528918 ) ) ;
#7784 = CARTESIAN_POINT ( 'NONE',  ( -10.51143808951550085, 11.41308718311005066, -231.3573069600382439 ) ) ;
#7785 = CARTESIAN_POINT ( 'NONE',  ( 14.98418162551161714, 4.450317369940187895, -227.9894155827521161 ) ) ;
#7786 = CARTESIAN_POINT ( 'NONE',  ( 0.000000000000000000, 0.000000000000000000, -75.00000000000000000 ) ) ;
#7787 = VERTEX_POINT ( 'NONE', #6193 ) ;
#7788 = CARTESIAN_POINT ( 'NONE',  ( -0.7292515499105728383, 28.18841485102515776, -220.8637599502617093 ) ) ;
#7789 = CARTESIAN_POINT ( 'NONE',  ( -16.05483997570105714, -7.226811045751038165, -218.5819178105544438 ) ) ;
#7790 = CARTESIAN_POINT ( 'NONE',  ( 15.42212722119060864, 5.401662248084913465, -220.8333402320903645 ) ) ;
#7791 = CARTESIAN_POINT ( 'NONE',  ( -3.771778814064143504, -12.72945944931849915, -225.7745976896340778 ) ) ;
#7792 = CIRCLE ( 'NONE', #14977, 22.56777165119825668 ) ;
#7793 = CARTESIAN_POINT ( 'NONE',  ( 19.38023697009521840, 2.464236985537108904, -223.2772968702357730 ) ) ;
#7794 = CARTESIAN_POINT ( 'NONE',  ( -14.69827142695382527, 14.49176359921644597, -217.9600391472806109 ) ) ;
#7795 = CARTESIAN_POINT ( 'NONE',  ( -3.000000000000030198, 0.000000000000000000, -105.0000000000000142 ) ) ;
#7796 = CARTESIAN_POINT ( 'NONE',  ( 12.12535264607833341, -6.902938132833007501, -227.3565233277489597 ) ) ;
#7797 = CARTESIAN_POINT ( 'NONE',  ( 9.214796078729456497, 26.59493510027307650, -225.5796848805584318 ) ) ;
#7798 = CARTESIAN_POINT ( 'NONE',  ( -17.78731991475362406, 16.78509880370027929, -218.2387321183659310 ) ) ;
#7799 = CARTESIAN_POINT ( 'NONE',  ( -12.36382104905844592, -0.1264132474004772688, -228.0034406263598896 ) ) ;
#7800 = CARTESIAN_POINT ( 'NONE',  ( -16.45250455720563210, -7.911775896682759601, -220.5271995834187067 ) ) ;
#7801 = CARTESIAN_POINT ( 'NONE',  ( 14.54999166170408209, 3.068772298969228096, -219.4784171371563275 ) ) ;
#7802 = CARTESIAN_POINT ( 'NONE',  ( 0.000000000000000000, 0.000000000000000000, 89.13175911166534604 ) ) ;
#7803 = CARTESIAN_POINT ( 'NONE',  ( -14.02432777873800518, -4.625777501976016559, -231.5673840409723709 ) ) ;
#7804 = CARTESIAN_POINT ( 'NONE',  ( -0.5888410438786807477, 14.99789765555501475, -227.7044550383138244 ) ) ;
#7805 = CARTESIAN_POINT ( 'NONE',  ( 28.65393683769942967, 4.398063292302325067, -219.1542358361629965 ) ) ;
#7806 = CARTESIAN_POINT ( 'NONE',  ( -6.593106361191484410, 26.27107262772703322, -231.8730401762632596 ) ) ;
#7807 = CARTESIAN_POINT ( 'NONE',  ( 5.501756899793208255, 15.97909684020861043, -233.9380718515096191 ) ) ;
#7808 = ORIENTED_EDGE ( 'NONE', *, *, #20402, .F. ) ;
#7809 = CARTESIAN_POINT ( 'NONE',  ( 7.465087220526423373, -26.16405931560015219, -221.3372167714960312 ) ) ;
#7810 = ORIENTED_EDGE ( 'NONE', *, *, #17232, .T. ) ;
#7811 = CARTESIAN_POINT ( 'NONE',  ( -1.380908993000753648, -20.21092959135559752, -218.0995018783601438 ) ) ;
#7812 = CARTESIAN_POINT ( 'NONE',  ( 14.19800769603076240, 4.587407146151301518, -224.2928935459285071 ) ) ;
#7813 = CARTESIAN_POINT ( 'NONE',  ( 16.07085865561684201, -17.65509622858733252, -216.6880805489183501 ) ) ;
#7814 = CARTESIAN_POINT ( 'NONE',  ( -28.30937415889876618, -7.921132361018833556, -222.9755670691803857 ) ) ;
#7815 = CARTESIAN_POINT ( 'NONE',  ( -12.14186164972853810, -9.217338937739926408, -220.4665480714278374 ) ) ;
#7816 = CARTESIAN_POINT ( 'NONE',  ( 3.746955526231565248, 25.82691596581962656, -220.7780764774678062 ) ) ;
#7817 = DIRECTION ( 'NONE',  ( 6.123233995736766036E-17, -0.000000000000000000, -1.000000000000000000 ) ) ;
#7818 = CARTESIAN_POINT ( 'NONE',  ( -21.39667546302236900, 3.687493526428279100, -235.1435990565495047 ) ) ;
#7819 = CARTESIAN_POINT ( 'NONE',  ( 6.093530912645064745, 16.79941505724243811, -232.1766444656230419 ) ) ;
#7820 = CARTESIAN_POINT ( 'NONE',  ( 8.321021197036545303, 25.59447019508656140, -228.6184429848799482 ) ) ;
#7821 = CARTESIAN_POINT ( 'NONE',  ( 11.86117213253061387, -14.68998886196529874, -215.0859965227146802 ) ) ;
#7822 = CARTESIAN_POINT ( 'NONE',  ( 26.59731715018858011, 13.56210517473685329, -229.5787264587298466 ) ) ;
#7823 = CARTESIAN_POINT ( 'NONE',  ( -14.22959263369750182, 18.28478771081826793, -217.8090497856120464 ) ) ;
#7824 = CARTESIAN_POINT ( 'NONE',  ( -16.40443871513620522, 4.023423476741658789, -228.9829044427089002 ) ) ;
#7825 = CARTESIAN_POINT ( 'NONE',  ( -0.1049609700611137120, -29.11428177772140558, -224.8408750893923411 ) ) ;
#7826 = DIRECTION ( 'NONE',  ( 0.000000000000000000, 0.000000000000000000, 1.000000000000000000 ) ) ;
#7827 = DIRECTION ( 'NONE',  ( 0.000000000000000000, 0.000000000000000000, 1.000000000000000000 ) ) ;
#7828 = CARTESIAN_POINT ( 'NONE',  ( 12.71450444683213021, 7.595266944807587350, -224.4213778964231665 ) ) ;
#7829 = CARTESIAN_POINT ( 'NONE',  ( 23.15933523859005660, -14.47549635653155775, -222.2572217030593436 ) ) ;
#7830 = FACE_OUTER_BOUND ( 'NONE', #16877, .T. ) ;
#7831 = CARTESIAN_POINT ( 'NONE',  ( -6.512931564893298386, -17.32529878264574563, -216.7284160531958719 ) ) ;
#7832 = PRODUCT_CONTEXT ( 'NONE', #16773, 'mechanical' ) ;
#7833 = CARTESIAN_POINT ( 'NONE',  ( -2.735889804569492600, 12.71735652435744512, -225.1194195722198117 ) ) ;
#7834 = CARTESIAN_POINT ( 'NONE',  ( -5.582510911615395699, 27.25430150734737111, -233.3200100877314469 ) ) ;
#7835 = ORIENTED_EDGE ( 'NONE', *, *, #12683, .F. ) ;
#7836 = CARTESIAN_POINT ( 'NONE',  ( -8.823862513872974489, 14.92351368520778898, -217.1499513473673346 ) ) ;
#7837 = CARTESIAN_POINT ( 'NONE',  ( -17.66047203424674450, -3.377913611064220056, -232.7782090104293786 ) ) ;
#7838 = CARTESIAN_POINT ( 'NONE',  ( -23.64367708099848286, -8.124846974203675742, 5.838821279329883041 ) ) ;
#7839 = DIRECTION ( 'NONE',  ( 1.000000000000000000, 0.000000000000000000, 0.000000000000000000 ) ) ;
#7840 = CARTESIAN_POINT ( 'NONE',  ( -11.98736441306973077, 11.45674391201457176, -217.8252237716743025 ) ) ;
#7841 = CARTESIAN_POINT ( 'NONE',  ( -3.608027314846280031, -12.96557536209330763, -219.9492366723279702 ) ) ;
#7842 = DIRECTION ( 'NONE',  ( -1.000000000000000000, 0.000000000000000000, 0.000000000000000000 ) ) ;
#7843 = CARTESIAN_POINT ( 'NONE',  ( -11.69688825528096388, 18.63404371591177622, -215.8612738028812714 ) ) ;
#7844 = CARTESIAN_POINT ( 'NONE',  ( -23.49520248890869212, 11.82830312093803649, -233.3871405502527807 ) ) ;
#7845 = ORIENTED_EDGE ( 'NONE', *, *, #14219, .F. ) ;
#7846 = CARTESIAN_POINT ( 'NONE',  ( -9.439286754415764591, 28.32957437491962338, -228.7842975624562598 ) ) ;
#7847 = CARTESIAN_POINT ( 'NONE',  ( -21.89065952084848021, -0.9940043559354364566, -216.9999999999999716 ) ) ;
#7848 = CARTESIAN_POINT ( 'NONE',  ( -12.79639481117843935, 1.974037863663017589, -229.6094308443170746 ) ) ;
#7849 = CARTESIAN_POINT ( 'NONE',  ( -7.103355004864593703, -14.30675315766165312, -225.9889059232917532 ) ) ;
#7850 = ORIENTED_EDGE ( 'NONE', *, *, #19047, .T. ) ;
#7851 = ADVANCED_FACE ( 'NONE', ( #19915 ), #19275, .T. ) ;
#7852 = CARTESIAN_POINT ( 'NONE',  ( 8.592982993077152187, 10.20906991731218838, -226.0923132092261483 ) ) ;
#7853 = CARTESIAN_POINT ( 'NONE',  ( 2.987882271643250931, 28.57355997650491020, -217.8917278841813925 ) ) ;
#7854 = CARTESIAN_POINT ( 'NONE',  ( -18.22136682449241363, -9.036057809225649606, -231.1742889867359736 ) ) ;
#7855 = DIRECTION ( 'NONE',  ( 0.000000000000000000, 0.000000000000000000, 1.000000000000000000 ) ) ;
#7856 = VERTEX_POINT ( 'NONE', #7188 ) ;
#7857 = CARTESIAN_POINT ( 'NONE',  ( 20.54442553493903389, -1.409480604460696007, -231.2888200459364327 ) ) ;
#7858 = CARTESIAN_POINT ( 'NONE',  ( -9.698809215651296611, -24.51491891025427350, -232.5150754403024962 ) ) ;
#7859 = CARTESIAN_POINT ( 'NONE',  ( 18.06016678184731461, 2.257982981100609354, -218.9983079406065940 ) ) ;
#7860 = CARTESIAN_POINT ( 'NONE',  ( -2.958555384449997661, 13.07587799061801093, -222.7767538261418565 ) ) ;
#7861 = CARTESIAN_POINT ( 'NONE',  ( 15.01641474852163505, -2.073694611913084351, -222.8298119658091139 ) ) ;
#7862 = UNCERTAINTY_MEASURE_WITH_UNIT (LENGTH_MEASURE( 1.000000000000000082E-05 ), #6764, 'distance_accuracy_value', 'NONE');
#7863 = CARTESIAN_POINT ( 'NONE',  ( -16.23590288079963173, 0.2625226423351309513, -226.8300841971807813 ) ) ;
#7864 = CARTESIAN_POINT ( 'NONE',  ( 7.174260007897984792, 9.971262771497068300, -226.2872513832048469 ) ) ;
#7865 = SURFACE_STYLE_FILL_AREA ( #6048 ) ;
#7866 = DIRECTION ( 'NONE',  ( 0.000000000000000000, 0.000000000000000000, 1.000000000000000000 ) ) ;
#7867 = CARTESIAN_POINT ( 'NONE',  ( 12.23063869552301242, 12.84118223717021934, -218.8273164334868284 ) ) ;
#7868 = CIRCLE ( 'NONE', #1031, 3.000000000000002665 ) ;
#7869 = CARTESIAN_POINT ( 'NONE',  ( 25.50000000000000000, -3.600000000000001421, -2.699999999999999289 ) ) ;
#7870 = CARTESIAN_POINT ( 'NONE',  ( 19.53765964318905546, -5.556987368099968627, -230.7409885362571345 ) ) ;
#7871 = CARTESIAN_POINT ( 'NONE',  ( -15.58529874627549461, -6.917566422457355202, -219.0138643999995054 ) ) ;
#7872 = DIRECTION ( 'NONE',  ( 0.000000000000000000, 0.000000000000000000, -1.000000000000000000 ) ) ;
#7873 = CARTESIAN_POINT ( 'NONE',  ( 0.000000000000000000, 0.000000000000000000, 93.00000000000000000 ) ) ;
#7874 = CARTESIAN_POINT ( 'NONE',  ( -5.383332542724544645, 15.12651309054520432, -231.5699995578976313 ) ) ;
#7875 = CARTESIAN_POINT ( 'NONE',  ( 24.73665505496147432, -17.48642391317526190, -218.9253764065177847 ) ) ;
#7876 = CARTESIAN_POINT ( 'NONE',  ( 22.36788034568564854, -2.140002702436959225, -217.7104380410378610 ) ) ;
#7877 = CARTESIAN_POINT ( 'NONE',  ( -21.28183200535960040, 1.085030287403131233, -217.0000000015322712 ) ) ;
#7878 = CARTESIAN_POINT ( 'NONE',  ( 28.03290210476798094, 13.48017620089690638, -224.9212082181537937 ) ) ;
#7879 = CARTESIAN_POINT ( 'NONE',  ( 8.858651440950676914, 22.47383302477780376, -230.7859943773311215 ) ) ;
#7880 = VERTEX_POINT ( 'NONE', #1586 ) ;
#7881 = CARTESIAN_POINT ( 'NONE',  ( 12.92460608403495037, -28.21656386930617089, -223.0937501850342812 ) ) ;
#7882 = CARTESIAN_POINT ( 'NONE',  ( 22.03647168420945590, 0.3315607655625663064, -232.0572713672586644 ) ) ;
#7883 = CARTESIAN_POINT ( 'NONE',  ( -3.687581766460184429, 30.01855770642711718, -218.8323691868875187 ) ) ;
#7884 = CARTESIAN_POINT ( 'NONE',  ( 3.641537757978871248, 12.43698445400491437, -220.3805014257186485 ) ) ;
#7885 = CARTESIAN_POINT ( 'NONE',  ( 14.06411491198613462, -8.094314315948059502, -222.2253600114596566 ) ) ;
#7886 = CARTESIAN_POINT ( 'NONE',  ( -3.514547081416551588, 30.38636916157537016, -227.3529586180979436 ) ) ;
#7887 = CARTESIAN_POINT ( 'NONE',  ( -10.84906991693323164, -9.635142796197690984, 93.00000000000001421 ) ) ;
#7888 = EDGE_CURVE ( 'NONE', #12432, #4133, #17849, .T. ) ;
#7889 = CARTESIAN_POINT ( 'NONE',  ( 2.291262277241625345, 17.20278591336981222, -216.2185160402476924 ) ) ;
#7890 = CARTESIAN_POINT ( 'NONE',  ( 13.72784977962315267, 2.687686193488206143, -220.8507880271885995 ) ) ;
#7891 = CARTESIAN_POINT ( 'NONE',  ( -20.54164754914381064, 7.122791156791981493, -233.5720402887671980 ) ) ;
#7892 = CARTESIAN_POINT ( 'NONE',  ( 24.42567939027770407, 10.22651298688739097, -219.4562066833365748 ) ) ;
#7893 = CARTESIAN_POINT ( 'NONE',  ( 9.094331215210646135, 23.85463374792894342, -219.7669638091879847 ) ) ;
#7894 = CARTESIAN_POINT ( 'NONE',  ( 1.387778780781446180E-13, -19.80000000000006111, 78.50000000000000000 ) ) ;
#7895 = EDGE_CURVE ( 'NONE', #13423, #21223, #5248, .T. ) ;
#7896 = EDGE_LOOP ( 'NONE', ( #4570, #14262 ) ) ;
#7897 = CARTESIAN_POINT ( 'NONE',  ( 11.16964468591631920, 25.71443501674299981, -224.7497461878887464 ) ) ;
#7898 = CARTESIAN_POINT ( 'NONE',  ( -16.39524763169126942, -10.97410814576847926, -232.9630882351523837 ) ) ;
#7899 = CARTESIAN_POINT ( 'NONE',  ( 25.80927844399814930, 11.21489550116160316, -221.3538377621514996 ) ) ;
#7900 = CARTESIAN_POINT ( 'NONE',  ( -0.07228948136920625156, -12.49432715273631445, -224.3346527204968766 ) ) ;
#7901 = PLANE ( 'NONE',  #5975 ) ;
#7902 = CARTESIAN_POINT ( 'NONE',  ( -15.82622499106666325, 9.895986579907866343, -218.5115209877527604 ) ) ;
#7903 = CARTESIAN_POINT ( 'NONE',  ( 8.767697218519710844, -14.65932909790238448, -230.8495237012982386 ) ) ;
#7904 = CARTESIAN_POINT ( 'NONE',  ( 9.931717191100288389, 12.93133689537362940, -228.8926047089119038 ) ) ;
#7905 = CARTESIAN_POINT ( 'NONE',  ( -13.93825237094548619, 9.044872709574327985, -220.1275804576921757 ) ) ;
#7906 = CARTESIAN_POINT ( 'NONE',  ( -12.02603758797190459, 8.152912069735307909, -218.2257190893353709 ) ) ;
#7907 = CARTESIAN_POINT ( 'NONE',  ( -18.92071285517992507, -7.235402657652117320, -230.6453433565968680 ) ) ;
#7908 = CARTESIAN_POINT ( 'NONE',  ( 8.463901354249619757, 8.457277735286822917, -222.5555366599873821 ) ) ;
#7909 = PLANE ( 'NONE',  #15572 ) ;
#7910 = CARTESIAN_POINT ( 'NONE',  ( -6.616223485457675579, -9.589312190179589024, -225.7195100648197581 ) ) ;
#7911 = CARTESIAN_POINT ( 'NONE',  ( 2.703362520412529779, 29.60004130108520215, -225.6165589735000481 ) ) ;
#7912 = CARTESIAN_POINT ( 'NONE',  ( 14.46993441875745390, 0.2699826811589002284, -230.0986938382904157 ) ) ;
#7913 = CARTESIAN_POINT ( 'NONE',  ( -5.786930954831501772, 15.78543306641166311, -231.0475152612371517 ) ) ;
#7914 = CARTESIAN_POINT ( 'NONE',  ( 3.490345297502855715, 11.17751288514984331, -224.7799703251421022 ) ) ;
#7915 = CARTESIAN_POINT ( 'NONE',  ( 2.737864789122675280, -26.51934750686404385, -230.0373452194950517 ) ) ;
#7916 = CARTESIAN_POINT ( 'NONE',  ( -0.8337089444836248697, -27.22572500676309559, -220.1932236949194532 ) ) ;
#7917 = EDGE_CURVE ( 'NONE', #2965, #2762, #20795, .T. ) ;
#7918 = CARTESIAN_POINT ( 'NONE',  ( -15.57331739480619248, 4.297375044201914740, -216.4079605712025511 ) ) ;
#7919 = CARTESIAN_POINT ( 'NONE',  ( 16.85953475301105442, -7.801609028127129086, -231.9437213283852941 ) ) ;
#7920 = CARTESIAN_POINT ( 'NONE',  ( -28.42127686227592420, -0.6461176296494712812, -221.6028628238154567 ) ) ;
#7921 = CARTESIAN_POINT ( 'NONE',  ( -12.04756914620937636, -13.80987496524771885, -232.8991007102355582 ) ) ;
#7922 = CARTESIAN_POINT ( 'NONE',  ( 2.659252340503933443, 26.58135124637517777, -228.4751214701929314 ) ) ;
#7923 =( NAMED_UNIT ( * ) PLANE_ANGLE_UNIT ( ) SI_UNIT ( $, .RADIAN. ) );
#7924 = CARTESIAN_POINT ( 'NONE',  ( -31.12406087576577463, 7.316399946619934092, -225.0171288978685027 ) ) ;
#7925 = CARTESIAN_POINT ( 'NONE',  ( -3.514547081416551588, 30.38636916157537016, -227.3529586180979436 ) ) ;
#7926 = CARTESIAN_POINT ( 'NONE',  ( 2.659252340503933443, 26.58135124637517777, -228.4751214701929314 ) ) ;
#7927 = CARTESIAN_POINT ( 'NONE',  ( 12.03076347463371398, -25.25364776008588308, -216.5688293904237298 ) ) ;
#7928 = CARTESIAN_POINT ( 'NONE',  ( 18.23116248274160256, 13.99874872632082123, -216.0593560670294835 ) ) ;
#7929 = CARTESIAN_POINT ( 'NONE',  ( -14.01525440049806193, 8.239250543314939890, -226.5804714421811070 ) ) ;
#7930 = CARTESIAN_POINT ( 'NONE',  ( -16.08005950484750102, -0.1764640578214327904, -223.5999988222837942 ) ) ;
#7931 = CARTESIAN_POINT ( 'NONE',  ( -5.322766963623397629, -16.65786661440869665, -219.3972027188067671 ) ) ;
#7932 = DIRECTION ( 'NONE',  ( 0.000000000000000000, 0.000000000000000000, -1.000000000000000000 ) ) ;
#7933 = DIRECTION ( 'NONE',  ( -1.000000000000000000, 0.000000000000000000, 0.000000000000000000 ) ) ;
#7934 = CARTESIAN_POINT ( 'NONE',  ( 13.61707622192329481, 14.84143455326118932, -217.6958999636067063 ) ) ;
#7935 = CARTESIAN_POINT ( 'NONE',  ( 15.35804315687698107, -7.528275283329426415, -228.0874909612831232 ) ) ;
#7936 = CARTESIAN_POINT ( 'NONE',  ( -25.44919589272258520, 4.740781954932180575, -232.0725131810460766 ) ) ;
#7937 = AXIS2_PLACEMENT_3D ( 'NONE', #626, #10656, #2089 ) ;
#7938 = CARTESIAN_POINT ( 'NONE',  ( -6.012234575298915473, -13.00555924700598709, -229.4955436083688483 ) ) ;
#7939 = CARTESIAN_POINT ( 'NONE',  ( 0.000000000000000000, 0.000000000000000000, 0.000000000000000000 ) ) ;
#7940 = CARTESIAN_POINT ( 'NONE',  ( -2.817219543927646175, 14.13981714106644993, -229.6779615865167443 ) ) ;
#7941 = CARTESIAN_POINT ( 'NONE',  ( 3.672031556878595282, 11.54613252248376831, -227.4694100414545801 ) ) ;
#7942 = ORIENTED_EDGE ( 'NONE', *, *, #9134, .T. ) ;
#7943 = CARTESIAN_POINT ( 'NONE',  ( -2.772442535524381579, 13.75675912271027457, -228.9770533867650215 ) ) ;
#7944 = CARTESIAN_POINT ( 'NONE',  ( -28.12632608809566293, -1.403418003803144742, -218.5233027210585988 ) ) ;
#7945 = CARTESIAN_POINT ( 'NONE',  ( -24.43287304230177881, -5.302030092552175056, 8.484947782864898258 ) ) ;
#7946 = DIRECTION ( 'NONE',  ( -1.000000000000000000, 0.000000000000000000, 0.000000000000000000 ) ) ;
#7947 = CARTESIAN_POINT ( 'NONE',  ( -10.51143808951550085, 11.41308718311005066, -231.3573069600382439 ) ) ;
#7948 = CARTESIAN_POINT ( 'NONE',  ( -10.19343904566850867, -16.03376756945627335, -215.1857286610140250 ) ) ;
#7949 = CARTESIAN_POINT ( 'NONE',  ( 27.92729748684602598, -8.572309054117944527, -222.6487661343338686 ) ) ;
#7950 = CARTESIAN_POINT ( 'NONE',  ( -9.540790481621398200, 9.981116473660406996, -228.6478862620407995 ) ) ;
#7951 = CARTESIAN_POINT ( 'NONE',  ( -24.69837543585720141, 12.57569301576483589, -232.4521327773205428 ) ) ;
#7952 = CARTESIAN_POINT ( 'NONE',  ( -3.130305314451475418, 18.08417128930788209, -217.9058652980469333 ) ) ;
#7953 = CARTESIAN_POINT ( 'NONE',  ( -21.08008464085897060, -0.9048411197481797119, -217.0000000010748522 ) ) ;
#7954 = CARTESIAN_POINT ( 'NONE',  ( 16.23850682336481199, 8.051046992137072422, -219.2473483181185827 ) ) ;
#7955 = CARTESIAN_POINT ( 'NONE',  ( -9.780669591740702273, -13.62818526938769104, -222.3368934028275135 ) ) ;
#7956 = VERTEX_POINT ( 'NONE', #20244 ) ;
#7957 = CARTESIAN_POINT ( 'NONE',  ( -22.04240660558204823, 19.10355008918698871, -223.9524535985323723 ) ) ;
#7958 = CARTESIAN_POINT ( 'NONE',  ( 12.98364502352995942, 13.67380631913144029, -233.1535077318696096 ) ) ;
#7959 = CARTESIAN_POINT ( 'NONE',  ( -2.328291070394212792, 14.80737693666302945, -219.0291440940735868 ) ) ;
#7960 = CARTESIAN_POINT ( 'NONE',  ( -14.27379873579015879, -4.865929470441826332, -223.9216412988620561 ) ) ;
#7961 = DIRECTION ( 'NONE',  ( 0.000000000000000000, 0.000000000000000000, -1.000000000000000000 ) ) ;
#7962 = ORIENTED_EDGE ( 'NONE', *, *, #5825, .T. ) ;
#7963 = CARTESIAN_POINT ( 'NONE',  ( -11.46843428684449151, 6.508406145394057596, -225.7212143570321814 ) ) ;
#7964 = CARTESIAN_POINT ( 'NONE',  ( -20.46754208161335598, -23.96478097336112256, -223.3311283152840758 ) ) ;
#7965 = FACE_OUTER_BOUND ( 'NONE', #21141, .T. ) ;
#7966 = CARTESIAN_POINT ( 'NONE',  ( 8.329997790135040603, 12.51216704542961899, -228.7022893680961602 ) ) ;
#7967 = DIRECTION ( 'NONE',  ( -1.000000000000000000, -0.000000000000000000, -0.000000000000000000 ) ) ;
#7968 = CARTESIAN_POINT ( 'NONE',  ( -15.61959985466312872, 8.133362592386543355, -230.7826037412100106 ) ) ;
#7969 = CARTESIAN_POINT ( 'NONE',  ( 14.65697969206133067, 11.40587726087447606, -233.3943609825344652 ) ) ;
#7970 = SURFACE_SIDE_STYLE ('',( #7865 ) ) ;
#7971 = AXIS2_PLACEMENT_3D ( 'NONE', #4312, #7932, #11195 ) ;
#7972 = CARTESIAN_POINT ( 'NONE',  ( 15.54915848664191280, 0.9682401509573658194, -222.1574103577552819 ) ) ;
#7973 = EDGE_CURVE ( 'NONE', #14896, #13719, #8140, .T. ) ;
#7974 = CARTESIAN_POINT ( 'NONE',  ( 12.58590500897257947, 11.38573988265384607, -230.4867078522624695 ) ) ;
#7975 = FACE_OUTER_BOUND ( 'NONE', #19124, .T. ) ;
#7976 = CARTESIAN_POINT ( 'NONE',  ( 22.17529396115045870, -12.37645153867399195, -229.8268438261158906 ) ) ;
#7977 = CARTESIAN_POINT ( 'NONE',  ( -14.93108815068229589, -1.792787290847115633, -227.6165763581034582 ) ) ;
#7978 = DIRECTION ( 'NONE',  ( 1.000000000000000000, 4.408728476930466911E-15, -0.000000000000000000 ) ) ;
#7979 = AXIS2_PLACEMENT_3D ( 'NONE', #19132, #8803, #7226 ) ;
#7980 = CARTESIAN_POINT ( 'NONE',  ( 21.99162546567091425, -2.693197373458130478E-15, -78.50000000000000000 ) ) ;
#7981 = CARTESIAN_POINT ( 'NONE',  ( -9.060295054034883222, 29.20313342278041802, -224.2979742714222482 ) ) ;
#7982 = CARTESIAN_POINT ( 'NONE',  ( 25.69869100782391413, -6.466588899411362057, -234.2905747065633193 ) ) ;
#7983 = CARTESIAN_POINT ( 'NONE',  ( 20.98776729843937972, -13.55153944770713359, -217.5092423276211946 ) ) ;
#7984 = CARTESIAN_POINT ( 'NONE',  ( -29.16153046926437753, 6.356672163541281506, -226.4393515956758165 ) ) ;
#7985 = CARTESIAN_POINT ( 'NONE',  ( 15.51129552754472307, 0.2180314803830030457, -231.3815478022924879 ) ) ;
#7986 = CARTESIAN_POINT ( 'NONE',  ( 18.30590144060498403, 15.06309558287673767, -219.0459394567220102 ) ) ;
#7987 = EDGE_LOOP ( 'NONE', ( #428, #1005, #5323, #17175 ) ) ;
#7988 = CARTESIAN_POINT ( 'NONE',  ( 3.722478027540565559, -17.18860102498078390, -232.3439289206262686 ) ) ;
#7989 = CARTESIAN_POINT ( 'NONE',  ( -10.16585704662448641, 10.34058050218014557, 93.00000000000000000 ) ) ;
#7990 = CARTESIAN_POINT ( 'NONE',  ( -21.73153953336191790, 8.758376218440917071, -235.2971293019126051 ) ) ;
#7991 = AXIS2_PLACEMENT_3D ( 'NONE', #7060, #7502, #1979 ) ;
#7992 = CARTESIAN_POINT ( 'NONE',  ( 9.818699534354031755, 13.69084898312510390, -233.4870046949650089 ) ) ;
#7993 = CARTESIAN_POINT ( 'NONE',  ( 4.065638640983322283, 32.08830473489500434, -226.0249194102539150 ) ) ;
#7994 = CARTESIAN_POINT ( 'NONE',  ( 26.42472234358771033, -2.855770380922216134, -231.8949512018254211 ) ) ;
#7995 = CARTESIAN_POINT ( 'NONE',  ( -3.643097910890548796, 22.16888955197135047, -233.9701981029593298 ) ) ;
#7996 = CARTESIAN_POINT ( 'NONE',  ( -13.11494368899652052, 3.355507568391938200, -225.9121440085824304 ) ) ;
#7997 = VECTOR ( 'NONE', #10345, 1000.000000000000000 ) ;
#7998 = CARTESIAN_POINT ( 'NONE',  ( -6.127117917506272882, 18.94558806480136681, -232.9763641438055117 ) ) ;
#7999 = CARTESIAN_POINT ( 'NONE',  ( -21.16281446184100545, 3.810576631694648775, -218.4455094643457187 ) ) ;
#8000 = CARTESIAN_POINT ( 'NONE',  ( -11.79584727357715934, 6.509288465425584036, -222.6080315736180921 ) ) ;
#8001 = CARTESIAN_POINT ( 'NONE',  ( 25.80927844399814930, 11.21489550116160316, -221.3538377621514996 ) ) ;
#8002 = CARTESIAN_POINT ( 'NONE',  ( 3.325336547283623378, 18.92213121405483633, -219.7480163085221818 ) ) ;
#8003 = CARTESIAN_POINT ( 'NONE',  ( -24.65069530437947876, -0.7989515219415058711, -216.4419420286324112 ) ) ;
#8004 = CARTESIAN_POINT ( 'NONE',  ( 8.856360819293511710, 14.24139612884802553, -227.7731680686805475 ) ) ;
#8005 = CARTESIAN_POINT ( 'NONE',  ( -9.294226473174397540, -12.00440878504259601, -219.6990993854437875 ) ) ;
#8006 = CARTESIAN_POINT ( 'NONE',  ( 12.23063869552301242, 12.84118223717021934, -218.8273164334868284 ) ) ;
#8007 = CARTESIAN_POINT ( 'NONE',  ( -8.373128421490182660, -27.12459427582015792, -230.7938890564172709 ) ) ;
#8008 = CIRCLE ( 'NONE', #10527, 4.500000000000000888 ) ;
#8009 = CARTESIAN_POINT ( 'NONE',  ( 21.30903826138442270, 0.6807850236355362794, -222.0732863424555035 ) ) ;
#8010 = EDGE_CURVE ( 'NONE', #16287, #1838, #3672, .T. ) ;
#8011 = AXIS2_PLACEMENT_3D ( 'NONE', #18224, #14521, #2784 ) ;
#8012 = CARTESIAN_POINT ( 'NONE',  ( -5.775873073292457249, 17.47547275616994256, -218.7209647771908578 ) ) ;
#8013 =( NAMED_UNIT ( * ) SI_UNIT ( $, .STERADIAN. ) SOLID_ANGLE_UNIT ( ) );
#8014 = CARTESIAN_POINT ( 'NONE',  ( 11.20610455198612598, -10.15455062626793037, -220.8168162286965526 ) ) ;
#8015 = CARTESIAN_POINT ( 'NONE',  ( 15.15306935214909778, 7.771180183537883757, -217.5526096523957165 ) ) ;
#8016 = CARTESIAN_POINT ( 'NONE',  ( -11.85645341316062051, 18.51497629668490674, -217.8828067666886454 ) ) ;
#8017 = CARTESIAN_POINT ( 'NONE',  ( -11.10150084103673684, 3.549415896002023896, -226.0408865487038952 ) ) ;
#8018 = CARTESIAN_POINT ( 'NONE',  ( -26.34963598119476913, -8.267085687785165504, -223.3493716711078889 ) ) ;
#8019 = CARTESIAN_POINT ( 'NONE',  ( -19.35155980425159683, 1.157993580480985552, -230.3698774940947942 ) ) ;
#8020 = DIRECTION ( 'NONE',  ( -1.000000000000000000, 0.000000000000000000, 0.000000000000000000 ) ) ;
#8021 = CARTESIAN_POINT ( 'NONE',  ( -21.30077981517617047, -23.37245693150986270, -228.9371924788557351 ) ) ;
#8022 = CARTESIAN_POINT ( 'NONE',  ( 14.69853173970351179, 23.44775873627089524, -231.2711109634281001 ) ) ;
#8023 = AXIS2_PLACEMENT_3D ( 'NONE', #16, #18596, #3268 ) ;
#8024 = CARTESIAN_POINT ( 'NONE',  ( 13.19406830060760605, 4.163358546877222288, -228.8532745215267425 ) ) ;
#8025 = AXIS2_PLACEMENT_3D ( 'NONE', #19180, #4200, #16041 ) ;
#8026 = CARTESIAN_POINT ( 'NONE',  ( 3.137667653003819446, 15.44806861187908176, -232.6841782316817842 ) ) ;
#8027 = CARTESIAN_POINT ( 'NONE',  ( 12.65306858828212810, 29.42930486385247590, -226.3758484992818012 ) ) ;
#8028 = VERTEX_POINT ( 'NONE', #11936 ) ;
#8029 = CARTESIAN_POINT ( 'NONE',  ( 4.568467666399979699, -17.52045581048442457, -219.7174082404806938 ) ) ;
#8030 = EDGE_LOOP ( 'NONE', ( #8652, #17878, #709, #21956 ) ) ;
#8031 = CARTESIAN_POINT ( 'NONE',  ( -5.980659577089002532, -19.45286470896024156, -217.9322865582606710 ) ) ;
#8032 = CARTESIAN_POINT ( 'NONE',  ( -22.61701582078733708, 5.416317966792455252, -214.6955127214549748 ) ) ;
#8033 = CARTESIAN_POINT ( 'NONE',  ( 12.84024077373997841, -14.50125846907313054, -216.8496453050001946 ) ) ;
#8034 = CARTESIAN_POINT ( 'NONE',  ( -24.25245498015852874, 0.2109992039763788352, -218.1398602137601301 ) ) ;
#8035 = CARTESIAN_POINT ( 'NONE',  ( -7.349743644505656093, -15.31718010764164539, -232.4470764718129772 ) ) ;
#8036 = CARTESIAN_POINT ( 'NONE',  ( 25.85827166240959940, 13.84420748389600675, -220.2831452073696425 ) ) ;
#8037 = CARTESIAN_POINT ( 'NONE',  ( -10.76972226383489506, 9.682563335906554158, -229.2555443445334333 ) ) ;
#8038 = CARTESIAN_POINT ( 'NONE',  ( 18.13412043358480474, 12.55378873098427128, -233.2186159706515696 ) ) ;
#8039 = CARTESIAN_POINT ( 'NONE',  ( -3.755296588130283553, 23.77975947300719284, -233.7323173085780752 ) ) ;
#8040 = CARTESIAN_POINT ( 'NONE',  ( 11.41090957555148222, 16.52772439454343711, -218.2458222691329013 ) ) ;
#8041 = CARTESIAN_POINT ( 'NONE',  ( 22.25403255790844881, -22.02690323431350450, -229.4561893391075671 ) ) ;
#8042 = AXIS2_PLACEMENT_3D ( 'NONE', #7318, #5498, #19229 ) ;
#8043 = AXIS2_PLACEMENT_3D ( 'NONE', #17298, #3334, #10216 ) ;
#8044 = CARTESIAN_POINT ( 'NONE',  ( 24.19635128940818447, 10.31396593861802380, -216.9479509989864425 ) ) ;
#8045 = CARTESIAN_POINT ( 'NONE',  ( -5.974114889119001681, 17.52937113675171332, -232.3862906442651592 ) ) ;
#8046 = CARTESIAN_POINT ( 'NONE',  ( -10.35216574861945560, -14.43870810227675605, -231.1876371800402126 ) ) ;
#8047 = CARTESIAN_POINT ( 'NONE',  ( 0.000000000000000000, 0.000000000000000000, 69.99999999999998579 ) ) ;
#8048 = DIRECTION ( 'NONE',  ( 0.1093404791528972547, -0.9940043559354329039, 0.000000000000000000 ) ) ;
#8049 = CARTESIAN_POINT ( 'NONE',  ( 12.85408565574548412, 7.821283853063205171, -223.1248833997948111 ) ) ;
#8050 = CARTESIAN_POINT ( 'NONE',  ( 11.03497432892593721, -13.14185978141811972, -229.3300340223075011 ) ) ;
#8051 = FACE_OUTER_BOUND ( 'NONE', #386, .T. ) ;
#8052 = EDGE_CURVE ( 'NONE', #3240, #8028, #3096, .T. ) ;
#8053 = CARTESIAN_POINT ( 'NONE',  ( -1.308474130992312023, -24.58654860180777391, -216.2430112183533026 ) ) ;
#8054 = EDGE_CURVE ( 'NONE', #11225, #20525, #14054, .T. ) ;
#8055 = CARTESIAN_POINT ( 'NONE',  ( -3.326157069579807946, 13.92020081821418565, -220.5733722327383930 ) ) ;
#8057 = CARTESIAN_POINT ( 'NONE',  ( -4.845359737286285551, 16.85396349487340117, -233.9229833851842670 ) ) ;
#8056 = AXIS2_PLACEMENT_3D ( 'NONE', #18326, #2453, #14732 ) ;
#8058 = ORIENTED_EDGE ( 'NONE', *, *, #14312, .F. ) ;
#8059 = CARTESIAN_POINT ( 'NONE',  ( 2.539761864897490007, 23.64215977235053501, -233.4645566207487661 ) ) ;
#8060 = CARTESIAN_POINT ( 'NONE',  ( 29.34815638429084927, -3.655059647784748122, -228.0165508611016207 ) ) ;
#8061 = CARTESIAN_POINT ( 'NONE',  ( 26.38334502096500245, -3.352420239867627494, -217.3603908026431384 ) ) ;
#8062 = DIRECTION ( 'NONE',  ( -1.000000000000000000, 0.000000000000000000, -0.000000000000000000 ) ) ;
#8063 = AXIS2_PLACEMENT_3D ( 'NONE', #18520, #10077, #8062 ) ;
#8064 = CARTESIAN_POINT ( 'NONE',  ( 5.017623471397871349, 29.83561274492976878, -222.9769172135417250 ) ) ;
#8065 = CARTESIAN_POINT ( 'NONE',  ( -10.13139158240655391, -23.04245082364802499, -234.6840773296079874 ) ) ;
#8066 = CARTESIAN_POINT ( 'NONE',  ( 6.741123954526870854, -14.00899218320067341, -219.0418835583997179 ) ) ;
#8067 = CARTESIAN_POINT ( 'NONE',  ( 18.55298002304457228, -12.22359628793950570, -216.9137843736221782 ) ) ;
#8068 = CARTESIAN_POINT ( 'NONE',  ( -17.17981675979428147, 1.478343374046288128, -216.2419730925687418 ) ) ;
#8069 = CARTESIAN_POINT ( 'NONE',  ( 15.20072702475037296, 19.31591084219522614, -219.7402199933931399 ) ) ;
#8070 = DIRECTION ( 'NONE',  ( 0.000000000000000000, 0.000000000000000000, -1.000000000000000000 ) ) ;
#8071 = CARTESIAN_POINT ( 'NONE',  ( -19.26845014167239611, 9.481468541508135672, -234.4856117705182328 ) ) ;
#8072 = CARTESIAN_POINT ( 'NONE',  ( -16.75383819933101748, -8.593015344009392820, -230.3978590765929084 ) ) ;
#8073 = ORIENTED_EDGE ( 'NONE', *, *, #4247, .F. ) ;
#8074 = CARTESIAN_POINT ( 'NONE',  ( -12.33203608746942237, 8.428128317385924717, -222.9277009507565026 ) ) ;
#8075 = CARTESIAN_POINT ( 'NONE',  ( 4.303123380281038024, 17.66787810618728827, -231.9745698734655832 ) ) ;
#8076 = CARTESIAN_POINT ( 'NONE',  ( -6.581016643627174645, 27.50493254600863935, -230.8763182197739070 ) ) ;
#8077 = CARTESIAN_POINT ( 'NONE',  ( -27.13703770709692265, -3.029478475984613173, -219.1636194202163779 ) ) ;
#8078 = DIRECTION ( 'NONE',  ( 0.000000000000000000, 0.000000000000000000, -1.000000000000000000 ) ) ;
#8079 = ORIENTED_EDGE ( 'NONE', *, *, #2038, .T. ) ;
#8080 = CARTESIAN_POINT ( 'NONE',  ( -12.31207293045244988, 6.732038552366256923, -221.0952066824360713 ) ) ;
#8081 = CARTESIAN_POINT ( 'NONE',  ( -14.91192530170583197, -15.94630704366669782, -215.1411503333790165 ) ) ;
#8082 = FACE_OUTER_BOUND ( 'NONE', #5781, .T. ) ;
#8083 = CARTESIAN_POINT ( 'NONE',  ( 6.093530912645064745, 16.79941505724243811, -232.1766444656230419 ) ) ;
#8084 = CARTESIAN_POINT ( 'NONE',  ( 26.00000000000000000, 1.360023205165816762E-13, 0.000000000000000000 ) ) ;
#8085 = UNCERTAINTY_MEASURE_WITH_UNIT (LENGTH_MEASURE( 1.000000000000000082E-05 ), #5060, 'distance_accuracy_value', 'NONE');
#8086 = CARTESIAN_POINT ( 'NONE',  ( 13.38839277810360429, -5.174145297632733786, -223.8523798909600941 ) ) ;
#8087 = CARTESIAN_POINT ( 'NONE',  ( -20.95553895916151177, 12.88782924195037438, -232.2493899712447956 ) ) ;
#8088 = CARTESIAN_POINT ( 'NONE',  ( 19.29259174080182504, 0.5828707127177102931, -219.2781652733668807 ) ) ;
#8089 = CARTESIAN_POINT ( 'NONE',  ( -24.49404684541703148, 5.034397176345765779, -8.664472460534662801 ) ) ;
#8090 = CARTESIAN_POINT ( 'NONE',  ( 21.30611872263680695, -0.6836234283288118441, -222.0738684573972819 ) ) ;
#8091 = FACE_OUTER_BOUND ( 'NONE', #13493, .T. ) ;
#8092 = CARTESIAN_POINT ( 'NONE',  ( 15.58552416334512536, -6.625011841737234342, -222.1645676924547104 ) ) ;
#8093 = CARTESIAN_POINT ( 'NONE',  ( -11.20272313682045073, -7.956653478762055087, -225.3025344850567819 ) ) ;
#8094 = CARTESIAN_POINT ( 'NONE',  ( -22.44689861640829776, -5.022254798600712000, 8.653524191425493228 ) ) ;
#8095 = CARTESIAN_POINT ( 'NONE',  ( -17.50000000000000711, 0.000000000000000000, -55.00000000000000000 ) ) ;
#8096 = CARTESIAN_POINT ( 'NONE',  ( -16.89013823391154290, 26.38860451648245231, -225.6449744083545852 ) ) ;
#8097 = CARTESIAN_POINT ( 'NONE',  ( 9.588041944343061118, -18.04984130968639633, -234.4334306750605776 ) ) ;
#8098 = CARTESIAN_POINT ( 'NONE',  ( 16.50235023187294203, -3.000022380394500310, -230.0447763498268614 ) ) ;
#8099 = CARTESIAN_POINT ( 'NONE',  ( -16.81936022032888545, 5.700806722825413786, -218.5726178058217215 ) ) ;
#8100 = CARTESIAN_POINT ( 'NONE',  ( 27.13894094332088969, 12.30518789341946295, -220.2765066586875093 ) ) ;
#8101 = CARTESIAN_POINT ( 'NONE',  ( 12.51085646230496273, 9.582567546749562126, -224.6200301875240939 ) ) ;
#8102 = ORIENTED_EDGE ( 'NONE', *, *, #12403, .F. ) ;
#8103 = CARTESIAN_POINT ( 'NONE',  ( 6.065954396161110651, -11.55577711821250553, -228.1182208427093485 ) ) ;
#8104 = DIRECTION ( 'NONE',  ( 1.000000000000000000, 0.000000000000000000, -0.000000000000000000 ) ) ;
#8105 = CARTESIAN_POINT ( 'NONE',  ( -19.86079186537285324, -0.7838168488858909821, -215.1601656726509475 ) ) ;
#8106 = CARTESIAN_POINT ( 'NONE',  ( 10.82528077991200810, 8.849546035972329250, -221.2068619981234008 ) ) ;
#8107 = CARTESIAN_POINT ( 'NONE',  ( -0.2269548806647709305, 12.31484924552052718, -228.6688778050056783 ) ) ;
#8108 = CARTESIAN_POINT ( 'NONE',  ( 20.48752708986941329, -13.44209471493726937, -230.9762584513030106 ) ) ;
#8109 = CARTESIAN_POINT ( 'NONE',  ( -2.934221234790329369, 15.07857928364152222, -230.9558365497803720 ) ) ;
#8110 = CARTESIAN_POINT ( 'NONE',  ( -26.02440924314744919, 2.824604386891162111, -232.0644005296583430 ) ) ;
#8111 = VECTOR ( 'NONE', #3694, 1000.000000000000000 ) ;
#8112 = CARTESIAN_POINT ( 'NONE',  ( 8.463901354249619757, 8.457277735286822917, -222.5555366599873821 ) ) ;
#8113 = MECHANICAL_DESIGN_GEOMETRIC_PRESENTATION_REPRESENTATION (  '', ( #9910 ), #9545 ) ;
#8114 = CARTESIAN_POINT ( 'NONE',  ( -26.88784739727922357, 10.07520213145270915, -227.1866063047054922 ) ) ;
#8115 = CARTESIAN_POINT ( 'NONE',  ( -3.514547081416551588, 30.38636916157537016, -227.3529586180979436 ) ) ;
#8116 = CARTESIAN_POINT ( 'NONE',  ( 22.84140515590350518, 18.29101041979067332, -226.2334522600520472 ) ) ;
#8117 = CARTESIAN_POINT ( 'NONE',  ( 3.433394806375676733, 19.92272173529517332, -219.3341428536850799 ) ) ;
#8118 = CARTESIAN_POINT ( 'NONE',  ( 14.64930099072384095, -2.233284345536625803, -226.6630761355773984 ) ) ;
#8119 = FACE_OUTER_BOUND ( 'NONE', #14390, .T. ) ;
#8120 = CARTESIAN_POINT ( 'NONE',  ( -18.11268275035277853, -3.459088653808292335, -218.4233329573673359 ) ) ;
#8121 = CARTESIAN_POINT ( 'NONE',  ( 13.43730899468209294, 8.427513769504761498, -221.4030804848920297 ) ) ;
#8122 = CARTESIAN_POINT ( 'NONE',  ( -2.170317331930874172, -31.11073952835316803, -223.3804330553629995 ) ) ;
#8123 = CARTESIAN_POINT ( 'NONE',  ( 18.89697753402894875, 2.884212079946345320, -225.8338386031039988 ) ) ;
#8124 = CARTESIAN_POINT ( 'NONE',  ( -17.14223598032838325, 23.31797360549976261, -226.5771676936548431 ) ) ;
#8125 =( NAMED_UNIT ( * ) PLANE_ANGLE_UNIT ( ) SI_UNIT ( $, .RADIAN. ) );
#8126 = CARTESIAN_POINT ( 'NONE',  ( 7.876378987416962296, -12.17572650474792617, -223.4643623724329018 ) ) ;
#8127 = CARTESIAN_POINT ( 'NONE',  ( 14.87635807518583775, 11.13002414557121789, -232.1789382499626981 ) ) ;
#8128 = CARTESIAN_POINT ( 'NONE',  ( -12.78923236353123727, 15.53885160143439315, -231.8946633672937878 ) ) ;
#8129 = CARTESIAN_POINT ( 'NONE',  ( -30.66857674073067130, 4.440060741118782239, -229.9901150862898476 ) ) ;
#8130 = CARTESIAN_POINT ( 'NONE',  ( -21.95460872137175201, -8.074699112730320039, -230.7190249947325071 ) ) ;
#8131 = VECTOR ( 'NONE', #21323, 1000.000000000000000 ) ;
#8132 = CARTESIAN_POINT ( 'NONE',  ( 21.75737151495493649, -2.205713500382455283, -233.2756072794337285 ) ) ;
#8133 = DIRECTION ( 'NONE',  ( -0.000000000000000000, -0.000000000000000000, -1.000000000000000000 ) ) ;
#8134 = CARTESIAN_POINT ( 'NONE',  ( -15.39182838237880446, -1.300641671086574469, -219.0680177603771597 ) ) ;
#8135 = CARTESIAN_POINT ( 'NONE',  ( 13.48097272627202159, 8.509510470709432894, -231.5257201610278059 ) ) ;
#8136 = CARTESIAN_POINT ( 'NONE',  ( -20.92673740658815973, 5.672885432599523270, -219.1433548642331459 ) ) ;
#8137 = EDGE_CURVE ( 'NONE', #10662, #12137, #12816, .T. ) ;
#8138 = CARTESIAN_POINT ( 'NONE',  ( 8.036750260989780514, 26.29729070384984624, -233.5018314387838529 ) ) ;
#8139 = CARTESIAN_POINT ( 'NONE',  ( 9.851209273476317918, 25.48401176094959553, -233.7173763849377792 ) ) ;
#8140 = CIRCLE ( 'NONE', #20705, 17.50000000000001066 ) ;
#8141 = CARTESIAN_POINT ( 'NONE',  ( -6.657868545208735611, -13.01156946085308874, -219.4730114480542227 ) ) ;
#8142 = ORIENTED_EDGE ( 'NONE', *, *, #6998, .F. ) ;
#8143 = CARTESIAN_POINT ( 'NONE',  ( 1.167080303844580058, -21.82675117811238152, -232.1335090276773485 ) ) ;
#8144 = CARTESIAN_POINT ( 'NONE',  ( -11.80036766549451599, 3.629178540272184783, -221.4826559383200220 ) ) ;
#8145 = CARTESIAN_POINT ( 'NONE',  ( 14.98777556431132219, -10.10815648641214004, -217.9795565018743844 ) ) ;
#8146 = CARTESIAN_POINT ( 'NONE',  ( 30.27398588404266633, 0.3550328743180605762, -224.9805995843073561 ) ) ;
#8147 = CARTESIAN_POINT ( 'NONE',  ( -23.84209965496292227, -7.976777114481962805, -232.1458837748831456 ) ) ;
#8148 = CARTESIAN_POINT ( 'NONE',  ( 10.97349919442152810, 9.416813005082010690, -227.3764328406868742 ) ) ;
#8149 = CARTESIAN_POINT ( 'NONE',  ( -25.00000000000001066, 0.000000000000000000, -224.9999999999999716 ) ) ;
#8150 = CARTESIAN_POINT ( 'NONE',  ( -11.83206531956964902, 10.60028422373495260, -231.1115289952381033 ) ) ;
#8151 = CARTESIAN_POINT ( 'NONE',  ( 10.59524789654300925, 9.532374763983630928, -223.0758647391057821 ) ) ;
#8152 = CARTESIAN_POINT ( 'NONE',  ( -2.808235066048971440, 30.42019778760651150, -222.6481917607299295 ) ) ;
#8153 = CARTESIAN_POINT ( 'NONE',  ( 13.64836464229338198, 15.83060743948028737, -232.0893758582176929 ) ) ;
#8154 = CARTESIAN_POINT ( 'NONE',  ( 20.24215890739238688, -18.92204689856563249, -233.5548650425709241 ) ) ;
#8155 = CARTESIAN_POINT ( 'NONE',  ( -12.89119823113977503, 10.10140484475961564, -218.5945808114896636 ) ) ;
#8156 = CARTESIAN_POINT ( 'NONE',  ( -1.406618399933933006, 16.47239985789244443, -232.2564017133012726 ) ) ;
#8157 = CARTESIAN_POINT ( 'NONE',  ( -12.60959727102843786, -12.64039607560028600, -218.2377899390859284 ) ) ;
#8158 = CARTESIAN_POINT ( 'NONE',  ( -26.58771759052039485, 5.114955214121561511, -218.2823714869195442 ) ) ;
#8159 = DIRECTION ( 'NONE',  ( 0.000000000000000000, 0.000000000000000000, 1.000000000000000000 ) ) ;
#8160 = CARTESIAN_POINT ( 'NONE',  ( 20.23125423326388628, 7.836699765464857137, -217.8891354894872450 ) ) ;
#8161 = CARTESIAN_POINT ( 'NONE',  ( 12.89891433044458502, -16.86700836158627936, -231.6320225002741040 ) ) ;
#8162 = CARTESIAN_POINT ( 'NONE',  ( -25.64868633208605786, 12.30364128039660798, -229.0020209687957049 ) ) ;
#8163 = EDGE_CURVE ( 'NONE', #7596, #16430, #11598, .T. ) ;
#8164 = CARTESIAN_POINT ( 'NONE',  ( -24.92024473536680773, -13.74570206812420103, -220.1598944320903115 ) ) ;
#8165 = CARTESIAN_POINT ( 'NONE',  ( -26.04932551096112192, 5.001193774903864409, -228.9498367494266802 ) ) ;
#8166 = CARTESIAN_POINT ( 'NONE',  ( 8.730612144237051453, 13.93563980088501886, -217.1627566045470132 ) ) ;
#8167 = ORIENTED_EDGE ( 'NONE', *, *, #17263, .T. ) ;
#8168 = CARTESIAN_POINT ( 'NONE',  ( 0.7245137624042983227, 13.44764381486384330, -223.4043886706536455 ) ) ;
#8169 = CARTESIAN_POINT ( 'NONE',  ( -29.90835019730369737, -3.078401082523886334, -228.7630230812432046 ) ) ;
#8170 = CARTESIAN_POINT ( 'NONE',  ( -23.70956031934304775, -7.931217015752231703, 6.099360975250686323 ) ) ;
#8171 = CARTESIAN_POINT ( 'NONE',  ( -22.63401512838757057, 0.000000000000000000, 77.51594804401857175 ) ) ;
#8172 = CARTESIAN_POINT ( 'NONE',  ( 1.382955251742491898, 16.46353944795171032, -231.7743150979565030 ) ) ;
#8173 = CARTESIAN_POINT ( 'NONE',  ( -3.316277044624852621, -11.89182204942354382, -222.3557635030381618 ) ) ;
#8174 = CARTESIAN_POINT ( 'NONE',  ( 8.532614294830283441, -28.73326933124977955, -229.1610356131385231 ) ) ;
#8175 = CARTESIAN_POINT ( 'NONE',  ( 17.43540344723615476, -3.335533435063737340, -230.8961756483947738 ) ) ;
#8176 = CARTESIAN_POINT ( 'NONE',  ( -27.17783334270200157, 15.20409188923851751, -223.6555185980277258 ) ) ;
#8177 = EDGE_CURVE ( 'NONE', #5555, #9014, #621, .T. ) ;
#8178 = CARTESIAN_POINT ( 'NONE',  ( 11.40028598017942230, 13.60807601628675023, -220.9105305289655519 ) ) ;
#8179 = CARTESIAN_POINT ( 'NONE',  ( -17.96792326766206926, -0.6237852504629022299, -217.9759415197746932 ) ) ;
#8180 = CARTESIAN_POINT ( 'NONE',  ( -18.17591565587962776, 16.23604867791855355, -233.2845329962925121 ) ) ;
#8181 = CARTESIAN_POINT ( 'NONE',  ( -16.76407561856198214, -10.47882714055132070, -219.0733374248486598 ) ) ;
#8182 = CARTESIAN_POINT ( 'NONE',  ( -16.12870690754239078, 23.19263481078822053, -221.6099859194323471 ) ) ;
#8183 = CARTESIAN_POINT ( 'NONE',  ( 10.88376588832297287, 7.577514201227793400, -222.7215714477710833 ) ) ;
#8184 = CARTESIAN_POINT ( 'NONE',  ( 1.867752180833619713, 31.25122076096762669, -227.4007918511463231 ) ) ;
#8185 = CARTESIAN_POINT ( 'NONE',  ( 12.74640035234706659, -6.767230903810586895, -221.4971111014800726 ) ) ;
#8186 = FACE_OUTER_BOUND ( 'NONE', #13352, .T. ) ;
#8187 = ORIENTED_EDGE ( 'NONE', *, *, #4639, .T. ) ;
#8188 = CARTESIAN_POINT ( 'NONE',  ( -18.39892766464214446, 25.11039525536027739, -225.3444503920457294 ) ) ;
#8189 = CARTESIAN_POINT ( 'NONE',  ( -3.077342110593487945, -14.65776296416898816, -220.8866639047373610 ) ) ;
#8190 = DIRECTION ( 'NONE',  ( 0.000000000000000000, 0.000000000000000000, 1.000000000000000000 ) ) ;
#8191 = CARTESIAN_POINT ( 'NONE',  ( 8.689059922489732912, 15.18271246186214363, -218.7354841152034908 ) ) ;
#8192 = CARTESIAN_POINT ( 'NONE',  ( 25.00000000000000000, 0.000000000000000000, 75.00000000000000000 ) ) ;
#8193 = CARTESIAN_POINT ( 'NONE',  ( 23.48720700658024896, -2.145453947144424500, -217.8824464111000054 ) ) ;
#8194 = CARTESIAN_POINT ( 'NONE',  ( -12.31207293045244988, 6.732038552366256923, -221.0952066824360713 ) ) ;
#8195 = CARTESIAN_POINT ( 'NONE',  ( -13.63002737749749826, 6.315035547785179837, -227.0490028799284516 ) ) ;
#8196 = CARTESIAN_POINT ( 'NONE',  ( 25.40954707198727647, 2.077273811637330159, -219.3610170479527426 ) ) ;
#8197 =( LENGTH_UNIT ( ) NAMED_UNIT ( * ) SI_UNIT ( .MILLI., .METRE. ) );
#8198 = CARTESIAN_POINT ( 'NONE',  ( 2.000000000000000000, 0.000000000000000000, -120.0000000000000142 ) ) ;
#8199 = CARTESIAN_POINT ( 'NONE',  ( 20.34032485158648029, 2.741617426884598530, -217.9827731991294968 ) ) ;
#8200 = DIRECTION ( 'NONE',  ( -1.000000000000000000, 0.000000000000000000, 0.000000000000000000 ) ) ;
#8201 = CARTESIAN_POINT ( 'NONE',  ( 23.20431681157275605, -3.694239143335118492, -219.1264243754107781 ) ) ;
#8202 = CARTESIAN_POINT ( 'NONE',  ( -14.48876282330270016, -2.056064607042531911, -223.6537127325441361 ) ) ;
#8203 = CARTESIAN_POINT ( 'NONE',  ( -21.17929482144447206, -8.972977884236303936, 4.463132373296485156 ) ) ;
#8204 = CARTESIAN_POINT ( 'NONE',  ( 0.000000000000000000, 0.000000000000000000, -78.50000000000000000 ) ) ;
#8205 = CARTESIAN_POINT ( 'NONE',  ( 8.132753622789847370, 14.44084924206385701, -222.7013822740049704 ) ) ;
#8206 = CARTESIAN_POINT ( 'NONE',  ( 11.85708236628466672, -10.49065743416967145, -217.1712987709648530 ) ) ;
#8207 = CARTESIAN_POINT ( 'NONE',  ( 6.374306683232226156, -13.38367253400339330, -219.9651431149896723 ) ) ;
#8208 = CARTESIAN_POINT ( 'NONE',  ( -13.51991436508781597, 16.61129329384914755, -232.1184346153593197 ) ) ;
#8209 = CARTESIAN_POINT ( 'NONE',  ( 14.50618777373884960, 4.375057440872940795, -230.8807389798650433 ) ) ;
#8210 = CARTESIAN_POINT ( 'NONE',  ( 24.96615890023450035, 5.871290975262302148, -218.1661911638112201 ) ) ;
#8211 = ORIENTED_EDGE ( 'NONE', *, *, #11247, .F. ) ;
#8212 = CARTESIAN_POINT ( 'NONE',  ( -7.069738587058329138, -16.45101055981254845, -220.5392980307454138 ) ) ;
#8213 = CARTESIAN_POINT ( 'NONE',  ( 0.000000000000000000, 21.00000000000006395, -75.00000000000000000 ) ) ;
#8214 = CARTESIAN_POINT ( 'NONE',  ( -11.10543627608095285, 3.497967533612860613, -224.1342318769322617 ) ) ;
#8215 = CARTESIAN_POINT ( 'NONE',  ( 11.78717493688862206, 28.63884142527983556, -229.7724827508652652 ) ) ;
#8216 = CARTESIAN_POINT ( 'NONE',  ( 3.044038000507106378, 30.22621415828681180, -231.1553244844465382 ) ) ;
#8217 = CARTESIAN_POINT ( 'NONE',  ( 28.84595539031434797, -3.450543886267656735, -229.1532420603894877 ) ) ;
#8218 = CARTESIAN_POINT ( 'NONE',  ( -2.735889804569492600, 12.71735652435744512, -225.1194195722198117 ) ) ;
#8219 = CARTESIAN_POINT ( 'NONE',  ( -11.79584727357715934, 6.509288465425584036, -222.6080315736180921 ) ) ;
#8220 = AXIS2_PLACEMENT_3D ( 'NONE', #6827, #13587, #1757 ) ;
#8221 = CARTESIAN_POINT ( 'NONE',  ( 11.38520239593705163, 18.87760105923376486, -235.3435298574111130 ) ) ;
#8222 = CARTESIAN_POINT ( 'NONE',  ( -26.91858181626453472, 10.72837452931393187, -223.4556356000267670 ) ) ;
#8223 = CARTESIAN_POINT ( 'NONE',  ( -1.249406995060579062, 25.48934319316224162, -216.9406480707515072 ) ) ;
#8224 = CARTESIAN_POINT ( 'NONE',  ( -6.688043756404080220, 8.469031667849378664, 92.00000000000001421 ) ) ;
#8225 = CARTESIAN_POINT ( 'NONE',  ( 15.50648685944955218, 24.16641006378193168, -224.4827813270165393 ) ) ;
#8226 = CARTESIAN_POINT ( 'NONE',  ( 22.14341918773124362, -7.622004812940091689, -217.4502831791021720 ) ) ;
#8227 = CARTESIAN_POINT ( 'NONE',  ( -17.50000000000000711, 0.000000000000000000, -60.00000000000000000 ) ) ;
#8228 = EDGE_CURVE ( 'NONE', #2762, #9014, #20357, .T. ) ;
#8229 = CARTESIAN_POINT ( 'NONE',  ( -26.98579662683621194, -8.531126968542736222, -229.5232528995939845 ) ) ;
#8230 = CARTESIAN_POINT ( 'NONE',  ( -21.89065952084861522, -0.9940043559354512226, -215.0000000000000000 ) ) ;
#8231 = CARTESIAN_POINT ( 'NONE',  ( -13.15060755141140980, -21.73659206351220519, -231.8601396556976226 ) ) ;
#8232 = CARTESIAN_POINT ( 'NONE',  ( 20.61940245508341363, 1.339931705218432079, -227.7063352817440318 ) ) ;
#8233 = CARTESIAN_POINT ( 'NONE',  ( -16.57767831947938575, 23.50485984366324388, -222.7977068309636763 ) ) ;
#8234 =( NAMED_UNIT ( * ) PLANE_ANGLE_UNIT ( ) SI_UNIT ( $, .RADIAN. ) );
#8235 = CARTESIAN_POINT ( 'NONE',  ( 13.17817051516727922, -26.22376201054615308, -223.3126545406654486 ) ) ;
#8236 = CARTESIAN_POINT ( 'NONE',  ( 16.73391517716289911, 11.95167056011791828, -233.0268722588312755 ) ) ;
#8237 = CARTESIAN_POINT ( 'NONE',  ( -4.142636420702924482, 14.17169704882741321, -225.1666440184957310 ) ) ;
#8239 = VECTOR ( 'NONE', #12142, 1000.000000000000000 ) ;
#8238 = CARTESIAN_POINT ( 'NONE',  ( -16.13584396029534318, 23.78382729893626646, -231.6788043429177435 ) ) ;
#8240 = ORIENTED_EDGE ( 'NONE', *, *, #17580, .T. ) ;
#8241 = CARTESIAN_POINT ( 'NONE',  ( -21.59231333450971135, -13.53975872187591989, -230.0942117760813517 ) ) ;
#8242 = CARTESIAN_POINT ( 'NONE',  ( 8.689059922489732912, 15.18271246186214363, -218.7354841152034908 ) ) ;
#8243 = CARTESIAN_POINT ( 'NONE',  ( -16.08005950484750102, -0.1764640578214327904, -223.5999988222837942 ) ) ;
#8244 = CARTESIAN_POINT ( 'NONE',  ( 0.000000000000000000, 0.000000000000000000, 95.00000000000000000 ) ) ;
#8245 = CARTESIAN_POINT ( 'NONE',  ( -27.06886705769815649, 1.548837563602061262, -218.3554811309518868 ) ) ;
#8246 = CARTESIAN_POINT ( 'NONE',  ( 8.821742718405863215, 10.82866050966069160, -221.4785132813277642 ) ) ;
#8247 = CARTESIAN_POINT ( 'NONE',  ( -18.46822229429615447, 3.027586163204024405, -230.1002726880134333 ) ) ;
#8248 = CARTESIAN_POINT ( 'NONE',  ( 2.068961274655788607, 15.13167107497539376, -217.8084559455312501 ) ) ;
#8249 = CARTESIAN_POINT ( 'NONE',  ( 16.10828274231666768, 3.530956590605524692, -220.6574330336208050 ) ) ;
#8250 = CARTESIAN_POINT ( 'NONE',  ( -10.99009178837907186, -10.32629327015668785, -231.8361825614163365 ) ) ;
#8251 = ORIENTED_EDGE ( 'NONE', *, *, #5979, .F. ) ;
#8252 = CARTESIAN_POINT ( 'NONE',  ( -17.01799258133205228, -17.74971190556693657, -217.5843211863294755 ) ) ;
#8253 = EDGE_CURVE ( 'NONE', #15223, #7787, #2028, .T. ) ;
#8254 = CARTESIAN_POINT ( 'NONE',  ( -25.32262741784088078, 2.623212696197013472, -234.6011982779809841 ) ) ;
#8255 = CARTESIAN_POINT ( 'NONE',  ( 8.532614294830283441, -28.73326933124977955, -229.1610356131385231 ) ) ;
#8256 = CARTESIAN_POINT ( 'NONE',  ( 27.71804559688024128, -15.88771542466010978, -225.5747850090131692 ) ) ;
#8257 = CARTESIAN_POINT ( 'NONE',  ( -17.21167111787709914, -1.850592482912338799, -230.8442569545952665 ) ) ;
#8258 = CARTESIAN_POINT ( 'NONE',  ( 11.44717363687632528, 10.34477785005100969, -220.4550508611108341 ) ) ;
#8259 = LINE ( 'NONE', #16921, #3775 ) ;
#8260 = CARTESIAN_POINT ( 'NONE',  ( -19.94037810645588138, 20.40093185429846656, -220.0593903119159620 ) ) ;
#8261 = CARTESIAN_POINT ( 'NONE',  ( 21.27834046766391651, 19.84195992785746654, -221.8454931627593965 ) ) ;
#8262 = CARTESIAN_POINT ( 'NONE',  ( 17.68508104102419409, 23.41266195669770767, -227.5327139115408954 ) ) ;
#8263 = CARTESIAN_POINT ( 'NONE',  ( 11.44717363687632528, 10.34477785005100969, -220.4550508611108341 ) ) ;
#8264 = CARTESIAN_POINT ( 'NONE',  ( 12.32676726801020450, -8.454629307895981327, -217.7935467833756036 ) ) ;
#8265 = CARTESIAN_POINT ( 'NONE',  ( -5.629016366058284149, 14.31889596247328633, -229.4177297515988414 ) ) ;
#8266 = CARTESIAN_POINT ( 'NONE',  ( 0.000000000000000000, 0.000000000000000000, -78.50000000000000000 ) ) ;
#8267 = CARTESIAN_POINT ( 'NONE',  ( 0.000000000000000000, 21.80000000000006111, -78.50000000000000000 ) ) ;
#8268 = CARTESIAN_POINT ( 'NONE',  ( 22.86997486125673618, 17.56009411325475966, -222.3578648042903296 ) ) ;
#8269 = CARTESIAN_POINT ( 'NONE',  ( 4.894111852004805030, -16.26971588820515890, -218.1545738548100530 ) ) ;
#8270 = CARTESIAN_POINT ( 'NONE',  ( -20.57288920227272655, 16.51351902378409520, -230.8484733908063333 ) ) ;
#8271 = CARTESIAN_POINT ( 'NONE',  ( 10.40160332990717151, 27.59713857063802323, -221.5374724512453213 ) ) ;
#8272 = CARTESIAN_POINT ( 'NONE',  ( -19.88402822078561627, -6.951120502836210413, -232.7962440186676361 ) ) ;
#8273 = CARTESIAN_POINT ( 'NONE',  ( 21.72366288329714834, 2.385777479048636351, -215.9150265590827757 ) ) ;
#8274 = CARTESIAN_POINT ( 'NONE',  ( 10.46530733675539793, 8.351728317179080818, -222.7431177495969621 ) ) ;
#8275 = CARTESIAN_POINT ( 'NONE',  ( -0.3969026096611234511, 20.89748314411456676, -216.3289738411752978 ) ) ;
#8276 = CARTESIAN_POINT ( 'NONE',  ( 18.71980393303116230, -12.14054210360577457, -231.5113610204687120 ) ) ;
#8277 = CARTESIAN_POINT ( 'NONE',  ( 25.09678678204237201, -16.96620885351193309, -225.7902784465786965 ) ) ;
#8278 = CARTESIAN_POINT ( 'NONE',  ( 1.526556658859590496E-13, -21.00000000000006040, 69.99999999999998579 ) ) ;
#8279 = CARTESIAN_POINT ( 'NONE',  ( 0.2389779871941385414, 16.64595486589868045, -218.1658233406367629 ) ) ;
#8280 = CARTESIAN_POINT ( 'NONE',  ( -12.86575055733568540, -10.70886189207742589, -216.1397835820578450 ) ) ;
#8281 = CARTESIAN_POINT ( 'NONE',  ( 11.14834367153813233, -21.42845646353120870, -216.4520112529555718 ) ) ;
#8282 = CARTESIAN_POINT ( 'NONE',  ( 15.65513449100897780, -26.00057195821942457, -227.4103383097017570 ) ) ;
#8283 = CARTESIAN_POINT ( 'NONE',  ( -8.463283775975803280, 12.69606588598396613, -228.6351674091961286 ) ) ;
#8284 = CARTESIAN_POINT ( 'NONE',  ( 12.16813927252146144, 18.27141895336136912, -230.9123895730235745 ) ) ;
#8285 = CARTESIAN_POINT ( 'NONE',  ( -24.48580119005125866, 9.312492396273500006, -232.5498413856076070 ) ) ;
#8286 = CARTESIAN_POINT ( 'NONE',  ( -13.34869474643618581, 6.516017165032126357, -231.2228057326931321 ) ) ;
#8287 = CARTESIAN_POINT ( 'NONE',  ( -11.98034293927688765, -10.98662817740026121, -223.7553339400932373 ) ) ;
#8288 = EDGE_CURVE ( 'NONE', #5604, #21305, #10669, .T. ) ;
#8289 = ORIENTED_EDGE ( 'NONE', *, *, #15957, .F. ) ;
#8290 = CARTESIAN_POINT ( 'NONE',  ( -9.627017372966443887, 15.60690227900018279, -218.8878023709062859 ) ) ;
#8291 = CARTESIAN_POINT ( 'NONE',  ( 12.74913679152205148, 9.185760885856177893, -218.6542381594888980 ) ) ;
#8292 = CARTESIAN_POINT ( 'NONE',  ( -6.415689407129693045, 29.32186846096819011, -228.3852515614991887 ) ) ;
#8293 = CLOSED_SHELL ( 'NONE', ( #4281, #17400, #9023, #10388, #20959, #20724, #13621, #10942, #19162, #1674, #14116, #3200, #10864, #4722, #18157, #10902, #22071, #21479, #5657, #11348, #5185, #19917, #9339, #15353, #18839, #5011, #9822, #7168, #8748, #3034, #21, #8972, #19678, #1033, #15864, #9155, #19715, #16574, #7321, #2121, #13110, #10313, #12571, #14783, #18288, #19004 ) ) ;
#8294 = CARTESIAN_POINT ( 'NONE',  ( 21.50885124049339936, -13.38680967545814404, -232.7305552638522954 ) ) ;
#8295 = CARTESIAN_POINT ( 'NONE',  ( 0.000000000000000000, 0.000000000000000000, -103.0000000000000000 ) ) ;
#8296 = VERTEX_POINT ( 'NONE', #425 ) ;
#8297 = APPLICATION_CONTEXT ( 'automotive_design' ) ;
#8298 = CARTESIAN_POINT ( 'NONE',  ( -19.00318367631585659, 13.14621133775862916, -233.8403879275295765 ) ) ;
#8299 = CARTESIAN_POINT ( 'NONE',  ( -9.514686225151438137, -9.899715435889788751, -219.6589915062491229 ) ) ;
#8300 = CARTESIAN_POINT ( 'NONE',  ( 25.50000000000000000, 0.5000000000000000000, -6.000000000000000000 ) ) ;
#8301 = CARTESIAN_POINT ( 'NONE',  ( 14.31308345469695453, 12.76656023072872159, -231.9445021321040770 ) ) ;
#8302 = DIRECTION ( 'NONE',  ( -2.891205793294678696E-17, 0.000000000000000000, -1.000000000000000000 ) ) ;
#8303 = CARTESIAN_POINT ( 'NONE',  ( 19.88636028791461641, -20.85574262981397453, -219.9907771812986823 ) ) ;
#8304 = CARTESIAN_POINT ( 'NONE',  ( -28.13472254077564116, 12.33996625515159629, -224.9141344439281909 ) ) ;
#8305 = CARTESIAN_POINT ( 'NONE',  ( -24.30769394037691100, 17.48612956801762053, -223.4340414801748693 ) ) ;
#8306 = CARTESIAN_POINT ( 'NONE',  ( 16.77055746703809191, 7.081497542956901370, -232.0295235404293521 ) ) ;
#8307 = CARTESIAN_POINT ( 'NONE',  ( -5.249799428260828904, -14.16826377401270065, -226.9124264195330056 ) ) ;
#8308 = CARTESIAN_POINT ( 'NONE',  ( 15.11539441383292903, 0.3024091369739423940, -222.0146986666484565 ) ) ;
#8309 = CARTESIAN_POINT ( 'NONE',  ( 28.51464931495100785, 5.422321182929326966, -223.8116416110474347 ) ) ;
#8310 = FACE_OUTER_BOUND ( 'NONE', #1629, .T. ) ;
#8311 = CARTESIAN_POINT ( 'NONE',  ( 15.75976565806011465, -3.644771625422815298, -224.1463364774561740 ) ) ;
#8312 = CARTESIAN_POINT ( 'NONE',  ( 13.35970348376145367, -2.045361282085617738, -227.1953586564414991 ) ) ;
#8313 = CARTESIAN_POINT ( 'NONE',  ( -19.63401512838747820, 0.000000000000000000, -77.51594804401857175 ) ) ;
#8314 = DIRECTION ( 'NONE',  ( -1.000000000000000000, -6.982962677686266711E-15, -0.000000000000000000 ) ) ;
#8315 = CARTESIAN_POINT ( 'NONE',  ( 11.27486163995310164, 25.12851252939060487, -222.6718455410222930 ) ) ;
#8316 = CARTESIAN_POINT ( 'NONE',  ( 13.13237050162318553, -11.26662123460813092, -216.1773046078333209 ) ) ;
#8317 = CARTESIAN_POINT ( 'NONE',  ( 13.49882595795384255, -9.201056071450322449, -219.2439763087855908 ) ) ;
#8318 = ORIENTED_EDGE ( 'NONE', *, *, #3078, .F. ) ;
#8319 = CARTESIAN_POINT ( 'NONE',  ( -15.51982305277792307, 19.76957551617798359, -231.4018974401358832 ) ) ;
#8320 = CARTESIAN_POINT ( 'NONE',  ( -22.10934047915413814, 0.9940043559354462266, -218.9999999999999716 ) ) ;
#8321 = CARTESIAN_POINT ( 'NONE',  ( 17.92683513449900445, 4.153309877386362814, -218.0960491240478234 ) ) ;
#8322 = ORIENTED_EDGE ( 'NONE', *, *, #315, .F. ) ;
#8323 = CARTESIAN_POINT ( 'NONE',  ( -6.842387616420496421, -14.58019248909694632, -223.2484495378617453 ) ) ;
#8324 = CARTESIAN_POINT ( 'NONE',  ( -0.1824719560092676052, -10.76782065184847959, 92.00000000000002842 ) ) ;
#8325 = CARTESIAN_POINT ( 'NONE',  ( -12.02603758797190459, 8.152912069735307909, -218.2257190893353709 ) ) ;
#8326 = CARTESIAN_POINT ( 'NONE',  ( 11.75630001506626776, 9.075791953625659048, -230.4239556728226717 ) ) ;
#8327 = CARTESIAN_POINT ( 'NONE',  ( 14.94332666820587008, -17.95933738324940165, -219.3037465242801147 ) ) ;
#8328 = CARTESIAN_POINT ( 'NONE',  ( 12.04687593227112430, 27.54339840196571743, -224.6466266724203820 ) ) ;
#8329 = CARTESIAN_POINT ( 'NONE',  ( -12.44873260470819787, 7.411970124596155785, -229.4214091473984070 ) ) ;
#8330 = EDGE_CURVE ( 'NONE', #3682, #19581, #239, .T. ) ;
#8331 = CARTESIAN_POINT ( 'NONE',  ( 22.92330650806121639, 19.11387742755395180, -231.6463539987045976 ) ) ;
#8332 = CARTESIAN_POINT ( 'NONE',  ( -16.29666348338687953, 2.994680995215331709, -221.2421885839926006 ) ) ;
#8333 = TOROIDAL_SURFACE ( 'NONE', #20898, 16.23205080756887853, 2.000000000000000000 ) ;
#8334 = CARTESIAN_POINT ( 'NONE',  ( -9.716674560061926869, 27.56227806819028103, -219.4917914922789919 ) ) ;
#8335 = CARTESIAN_POINT ( 'NONE',  ( -7.484971844052076939, 7.743026158993130181, 91.99999999999998579 ) ) ;
#8336 = CARTESIAN_POINT ( 'NONE',  ( 3.060417506408009469, 27.46204888741655026, -226.6022202862033623 ) ) ;
#8337 = PLANE ( 'NONE',  #15914 ) ;
#8338 = CARTESIAN_POINT ( 'NONE',  ( -21.00000000000008171, 0.000000000000000000, -60.00000000000001421 ) ) ;
#8339 = PRODUCT_DEFINITION_SHAPE ( 'NONE', 'NONE',  #17443 ) ;
#8340 = CARTESIAN_POINT ( 'NONE',  ( -25.42089018817326007, -6.263968923056941307, -218.6542964065910439 ) ) ;
#8341 = CARTESIAN_POINT ( 'NONE',  ( -30.17036082276531772, 5.959165309317525860, -219.4883053239162791 ) ) ;
#8342 = CARTESIAN_POINT ( 'NONE',  ( -12.60888841760081824, -15.87650330583304914, -218.3826098682522456 ) ) ;
#8343 = CARTESIAN_POINT ( 'NONE',  ( 21.56647080447661224, 0.4294288297056144676, -227.9703514235376076 ) ) ;
#8344 = AXIS2_PLACEMENT_3D ( 'NONE', #1205, #9653, #1091 ) ;
#8345 = CARTESIAN_POINT ( 'NONE',  ( -10.70754874174748039, 23.84972878377777405, -230.7991598016655246 ) ) ;
#8346 = CARTESIAN_POINT ( 'NONE',  ( 11.75796858304313375, -24.75965012883946414, -219.8219186532837455 ) ) ;
#8347 = CARTESIAN_POINT ( 'NONE',  ( 12.89118769162836031, 6.140251663080722899, -228.8792332048833771 ) ) ;
#8348 = CARTESIAN_POINT ( 'NONE',  ( -4.490213599459100813, 14.55066867058898694, -222.6488251579668827 ) ) ;
#8349 = CARTESIAN_POINT ( 'NONE',  ( -16.38161496430853248, 17.22219235543852989, -215.3343469598664797 ) ) ;
#8350 = VERTEX_POINT ( 'NONE', #17645 ) ;
#8351 = CARTESIAN_POINT ( 'NONE',  ( 18.88835481822873774, -3.841660717124094848, -234.8883833189080974 ) ) ;
#8352 = EDGE_LOOP ( 'NONE', ( #17790, #9423, #3549, #1528 ) ) ;
#8353 = CARTESIAN_POINT ( 'NONE',  ( 10.85888002857596923, 15.81835858589122878, -232.3913150909872627 ) ) ;
#8354 = CARTESIAN_POINT ( 'NONE',  ( -14.08236938285573636, 6.062428076406559008, -221.7923619418395447 ) ) ;
#8355 = CARTESIAN_POINT ( 'NONE',  ( -21.16281446184100545, 3.810576631694648775, -218.4455094643457187 ) ) ;
#8356 = CIRCLE ( 'NONE', #6181, 12.50000000000000355 ) ;
#8357 = CARTESIAN_POINT ( 'NONE',  ( 14.96415947227435339, -1.927366939720012606, -222.7010313878448358 ) ) ;
#8358 = CARTESIAN_POINT ( 'NONE',  ( 28.33476664927451338, -0.7768526459456059907, -228.3750448408243869 ) ) ;
#8359 = CARTESIAN_POINT ( 'NONE',  ( 13.82984244654956107, 22.51831320572884820, -232.1830460045772213 ) ) ;
#8360 = CARTESIAN_POINT ( 'NONE',  ( -15.50322565568834321, 9.749075856218723857, -229.6019304695566916 ) ) ;
#8361 = CARTESIAN_POINT ( 'NONE',  ( -6.415689407129693045, 29.32186846096819011, -228.3852515614991887 ) ) ;
#8362 = CARTESIAN_POINT ( 'NONE',  ( 14.68015846516680867, 2.651775288685355836, -224.1317433549420173 ) ) ;
#8363 = CARTESIAN_POINT ( 'NONE',  ( -3.607128793317693649, -14.45447024314366402, -228.6383918289709811 ) ) ;
#8364 = CIRCLE ( 'NONE', #3316, 25.52219491023488018 ) ;
#8365 = VERTEX_POINT ( 'NONE', #7736 ) ;
#8366 = CARTESIAN_POINT ( 'NONE',  ( -8.983992482398329926, -13.08794618741998761, -229.3325301586503713 ) ) ;
#8367 = CARTESIAN_POINT ( 'NONE',  ( -15.35982698007958724, 5.508237851081846159, -233.6994028941782631 ) ) ;
#8368 = CARTESIAN_POINT ( 'NONE',  ( 2.513843158659109456, -14.78137297724497401, -219.3443999184743518 ) ) ;
#8369 = CARTESIAN_POINT ( 'NONE',  ( -0.9414827276148034496, 23.96885519606619752, -216.4491898092606164 ) ) ;
#8370 = CARTESIAN_POINT ( 'NONE',  ( 14.18953136290653205, -9.569333121228954298, -216.2179364387266389 ) ) ;
#8371 = CARTESIAN_POINT ( 'NONE',  ( -14.40111287326894640, -6.123720356435734757, -220.5571602876142094 ) ) ;
#8372 = CARTESIAN_POINT ( 'NONE',  ( 24.20411255886326529, 12.66254860825103634, -218.0144359054998802 ) ) ;
#8373 = DIRECTION ( 'NONE',  ( -1.000000000000000000, -0.000000000000000000, -0.000000000000000000 ) ) ;
#8374 = PRODUCT_DEFINITION ( 'UNKNOWN', '', #12463, #14834 ) ;
#8375 = CARTESIAN_POINT ( 'NONE',  ( -13.96653539523557619, 20.94398119165846239, -231.8597527081015528 ) ) ;
#8376 = CARTESIAN_POINT ( 'NONE',  ( 16.82251835652528982, 18.18719385133374544, -231.8032941011735772 ) ) ;
#8377 = CARTESIAN_POINT ( 'NONE',  ( 8.329997790135040603, 12.51216704542961899, -228.7022893680961602 ) ) ;
#8378 = CARTESIAN_POINT ( 'NONE',  ( 9.253909228257674258, 17.69332415812615977, -230.9900471521432621 ) ) ;
#8379 = CARTESIAN_POINT ( 'NONE',  ( -0.3220389361364618397, -21.73025720764451663, -234.5721229173148856 ) ) ;
#8380 = CARTESIAN_POINT ( 'NONE',  ( -12.33583941212908108, 22.27382123621224608, -231.6290720151527296 ) ) ;
#8381 = CARTESIAN_POINT ( 'NONE',  ( -25.29098058636142810, 5.014641116111857144, -217.4658967307323110 ) ) ;
#8382 = TOROIDAL_SURFACE ( 'NONE', #12346, 24.63401512838747820, 3.000000000000000888 ) ;
#8383 = DIRECTION ( 'NONE',  ( 0.000000000000000000, 0.000000000000000000, 1.000000000000000000 ) ) ;
#8384 = CIRCLE ( 'NONE', #13780, 10.00000000000000000 ) ;
#8385 = DIRECTION ( 'NONE',  ( 0.000000000000000000, 0.000000000000000000, -1.000000000000000000 ) ) ;
#8386 = CARTESIAN_POINT ( 'NONE',  ( 8.168748216644726057, -13.67612414567523693, -220.8005964828080607 ) ) ;
#8387 = CARTESIAN_POINT ( 'NONE',  ( -11.94782396647286049, 8.456988817430419303, -225.5094493096559063 ) ) ;
#8388 = CARTESIAN_POINT ( 'NONE',  ( 2.464084843620814702, 29.35663482419208492, -227.0015060686748143 ) ) ;
#8389 = CARTESIAN_POINT ( 'NONE',  ( -22.53818779203657741, -7.663114047788936567, -232.6164956747681458 ) ) ;
#8390 = CARTESIAN_POINT ( 'NONE',  ( 13.30790133003807441, 0.6370684082013071681, -222.3495379725305270 ) ) ;
#8391 = CARTESIAN_POINT ( 'NONE',  ( 15.88965480228581839, 12.37830464553330678, -233.8570207506254235 ) ) ;
#8392 = VERTEX_POINT ( 'NONE', #3902 ) ;
#8393 = CARTESIAN_POINT ( 'NONE',  ( 5.248230734842167955, 23.54336384919183445, -216.8914391693808739 ) ) ;
#8394 = CARTESIAN_POINT ( 'NONE',  ( 15.59528062753244804, -5.679035096727840681, -230.0190217829878918 ) ) ;
#8395 = CARTESIAN_POINT ( 'NONE',  ( 14.49023023880111083, -12.14520762395643061, -217.6171285705176501 ) ) ;
#8396 = CARTESIAN_POINT ( 'NONE',  ( -2.000000000000000000, 2.449293598294706414E-16, -120.0000000000000142 ) ) ;
#8397 = CARTESIAN_POINT ( 'NONE',  ( 8.979547488457603421, 23.24376652602565230, -232.6628827740196357 ) ) ;
#8398 = CARTESIAN_POINT ( 'NONE',  ( -27.95235446785429545, -6.124178816625678756, -218.3296603670965226 ) ) ;
#8399 = CARTESIAN_POINT ( 'NONE',  ( -13.13432812001650341, -19.42279346457301514, -216.4126494286626610 ) ) ;
#8400 = CARTESIAN_POINT ( 'NONE',  ( 10.30328786010431052, -20.08430705480546408, -216.1847100135515802 ) ) ;
#8401 = AXIS2_PLACEMENT_3D ( 'NONE', #83, #12016, #4919 ) ;
#8402 = CARTESIAN_POINT ( 'NONE',  ( -10.10782416658048710, 9.083762506436128703, -227.1045422723873344 ) ) ;
#8403 = CARTESIAN_POINT ( 'NONE',  ( 5.112468059216026539, 15.05346046978967856, -223.6558835435016590 ) ) ;
#8404 = CARTESIAN_POINT ( 'NONE',  ( -13.69675006931110417, 3.702342960760605539, -228.0723273272095355 ) ) ;
#8405 = CARTESIAN_POINT ( 'NONE',  ( -20.49711526797010208, 7.006997077916217620, -215.3369776077118445 ) ) ;
#8406 = CARTESIAN_POINT ( 'NONE',  ( -22.73111095712577168, -10.24355154293710690, -230.8570942615963872 ) ) ;
#8407 = VERTEX_POINT ( 'NONE', #3791 ) ;
#8408 = CARTESIAN_POINT ( 'NONE',  ( -4.073886805163430935, 14.35067061637828623, -226.4733297826468572 ) ) ;
#8409 = CARTESIAN_POINT ( 'NONE',  ( 23.18902850759750933, 20.27908137164207147, -226.2847847834817117 ) ) ;
#8410 = CARTESIAN_POINT ( 'NONE',  ( 19.07698357483942786, 25.86742807064150895, -222.6991278896559834 ) ) ;
#8411 = CARTESIAN_POINT ( 'NONE',  ( 10.62272209279942992, -9.818939940036045755, -222.1403336352628344 ) ) ;
#8412 = CARTESIAN_POINT ( 'NONE',  ( -23.00000000000000000, 0.000000000000000000, -30.00000000000000000 ) ) ;
#8413 = ORIENTED_EDGE ( 'NONE', *, *, #1949, .T. ) ;
#8414 = CARTESIAN_POINT ( 'NONE',  ( -4.104500432947460808, 15.73223271406093460, -218.0734292856946297 ) ) ;
#8415 = CARTESIAN_POINT ( 'NONE',  ( -19.52111408301234974, -15.33805657151784985, -234.6553009392178808 ) ) ;
#8416 = DIRECTION ( 'NONE',  ( 0.000000000000000000, 0.000000000000000000, -1.000000000000000000 ) ) ;
#8417 = CARTESIAN_POINT ( 'NONE',  ( 20.41153371889344825, 17.18812948447019551, -230.7531656956970778 ) ) ;
#8418 = CARTESIAN_POINT ( 'NONE',  ( 0.000000000000000000, 0.000000000000000000, 75.00000000000000000 ) ) ;
#8419 = CARTESIAN_POINT ( 'NONE',  ( 24.96294718070021901, -13.86220829677249178, -229.4442241490162075 ) ) ;
#8420 =( LENGTH_UNIT ( ) NAMED_UNIT ( * ) SI_UNIT ( .MILLI., .METRE. ) );
#8421 = CARTESIAN_POINT ( 'NONE',  ( -13.11494368899652052, 3.355507568391938200, -225.9121440085824304 ) ) ;
#8422 = EDGE_CURVE ( 'NONE', #19105, #14415, #20344, .T. ) ;
#8423 = CARTESIAN_POINT ( 'NONE',  ( 15.70515172005171323, -0.7403987186381333352, -226.4590404369862995 ) ) ;
#8424 = CARTESIAN_POINT ( 'NONE',  ( -12.50828242918857036, -25.45147276965577277, -228.7626325223041022 ) ) ;
#8425 = DIRECTION ( 'NONE',  ( -1.000000000000000000, 0.000000000000000000, 0.000000000000000000 ) ) ;
#8426 = CARTESIAN_POINT ( 'NONE',  ( 14.80394259695730064, 1.224172658189580432, -225.4564070658925061 ) ) ;
#8427 = CARTESIAN_POINT ( 'NONE',  ( -16.20072894238734307, 0.5024448614660336210, -230.4554067149722130 ) ) ;
#8428 = CARTESIAN_POINT ( 'NONE',  ( 11.61478720377483675, -14.40087791365289860, -230.4552745109343448 ) ) ;
#8429 = CARTESIAN_POINT ( 'NONE',  ( 13.59365628422294137, -1.921009172773990858, -227.3069749406489564 ) ) ;
#8430 = FACE_OUTER_BOUND ( 'NONE', #19282, .T. ) ;
#8431 = CARTESIAN_POINT ( 'NONE',  ( 10.79895562092076844, 12.01490073542734116, -225.7380208924852809 ) ) ;
#8432 = CARTESIAN_POINT ( 'NONE',  ( 5.112468059216026539, 15.05346046978967856, -223.6558835435016590 ) ) ;
#8433 = CARTESIAN_POINT ( 'NONE',  ( 10.18197402670511842, -10.22146582328408115, -231.5691222609812598 ) ) ;
#8434 = CARTESIAN_POINT ( 'NONE',  ( 12.13827923251525220, -9.172799829723585319, -229.1860353116090891 ) ) ;
#8435 = CARTESIAN_POINT ( 'NONE',  ( -16.12870690754239078, 23.19263481078822053, -221.6099859194323471 ) ) ;
#8436 = CARTESIAN_POINT ( 'NONE',  ( -15.65611835717891687, 5.486779671999271635, -227.0554626315911264 ) ) ;
#8437 = CARTESIAN_POINT ( 'NONE',  ( 15.80790828609669951, 3.698719088746416972, -219.8106174092292804 ) ) ;
#8438 = EDGE_LOOP ( 'NONE', ( #46, #9710, #2656, #15221 ) ) ;
#8439 = AXIS2_PLACEMENT_3D ( 'NONE', #5354, #5589, #20772 ) ;
#8440 = CARTESIAN_POINT ( 'NONE',  ( -7.194605141218047173, -25.04260655977047278, -230.2952862975163271 ) ) ;
#8441 = CARTESIAN_POINT ( 'NONE',  ( 9.716662759434166574, -5.484269832949179246, 92.00000000000002842 ) ) ;
#8442 = CARTESIAN_POINT ( 'NONE',  ( -13.55637112341987383, 4.614880311503475774, -231.8130385267184010 ) ) ;
#8443 = ORIENTED_EDGE ( 'NONE', *, *, #19047, .F. ) ;
#8444 = CARTESIAN_POINT ( 'NONE',  ( 10.39636392256998221, 18.46527700675686035, -215.1860221565626148 ) ) ;
#8445 = CARTESIAN_POINT ( 'NONE',  ( 16.48523685932656235, -13.39871719616043855, -218.9387417542926926 ) ) ;
#8446 = CARTESIAN_POINT ( 'NONE',  ( 2.539761864897490007, 23.64215977235053501, -233.4645566207487661 ) ) ;
#8447 = CARTESIAN_POINT ( 'NONE',  ( -28.17543631911187063, 3.557555778861649642, -230.1980773687482156 ) ) ;
#8448 = CARTESIAN_POINT ( 'NONE',  ( 25.17176037151762813, 18.95054595444721102, -221.3490360113488862 ) ) ;
#8449 = ADVANCED_FACE ( 'NONE', ( #12579, #17871 ), #19422, .F. ) ;
#8450 = CARTESIAN_POINT ( 'NONE',  ( -19.84402263676350131, 8.565754689849573111, -217.6561116767911983 ) ) ;
#8451 = CARTESIAN_POINT ( 'NONE',  ( -0.3969026096611234511, 20.89748314411456676, -216.3289738411752978 ) ) ;
#8452 = AXIS2_PLACEMENT_3D ( 'NONE', #4888, #1072, #19966 ) ;
#8453 = CARTESIAN_POINT ( 'NONE',  ( 1.665334536937735316E-13, -24.63401512838760610, -77.51594804401857175 ) ) ;
#8454 = CARTESIAN_POINT ( 'NONE',  ( 8.332496243628455090, -29.79192972398156769, -226.1452587264855367 ) ) ;
#8455 =( GEOMETRIC_REPRESENTATION_CONTEXT ( 3 ) GLOBAL_UNCERTAINTY_ASSIGNED_CONTEXT ( ( #2227 ) ) GLOBAL_UNIT_ASSIGNED_CONTEXT ( ( #7286, #8751, #7399 ) ) REPRESENTATION_CONTEXT ( 'NONE', 'WORKASPACE' ) );
#8456 = CARTESIAN_POINT ( 'NONE',  ( 17.43540344723615476, -3.335533435063737340, -230.8961756483947738 ) ) ;
#8457 = CARTESIAN_POINT ( 'NONE',  ( 0.000000000000000000, 0.000000000000000000, 75.00000000000000000 ) ) ;
#8458 = CARTESIAN_POINT ( 'NONE',  ( -27.85133024402786006, -1.794102530182491773, -229.4204807338591081 ) ) ;
#8459 = CARTESIAN_POINT ( 'NONE',  ( 15.52719855059926424, 1.633696074270991172, -221.7349885876216433 ) ) ;
#8460 = CARTESIAN_POINT ( 'NONE',  ( -22.37826137345437871, -13.90312800710061047, -229.3506127454622572 ) ) ;
#8461 = CARTESIAN_POINT ( 'NONE',  ( 18.76166303929371537, 3.000000000000002665, -224.9999999999997442 ) ) ;
#8462 = SHAPE_REPRESENTATION ( '360-Degree Detachable Power Base', ( #6677 ), #10247 ) ;
#8463 = CARTESIAN_POINT ( 'NONE',  ( 12.20621255000322947, -21.57429421806300240, -232.1397031738524674 ) ) ;
#8464 = EDGE_CURVE ( 'NONE', #5173, #3103, #4630, .T. ) ;
#8465 = CARTESIAN_POINT ( 'NONE',  ( -15.30864812529618391, 1.596444765892653717, -220.3859421844601627 ) ) ;
#8466 = CARTESIAN_POINT ( 'NONE',  ( -14.22255565734842619, 21.32307452572284134, -218.8849463683180261 ) ) ;
#8467 = CARTESIAN_POINT ( 'NONE',  ( -4.591517861330576267, 12.55780501983563191, -223.5932882008353033 ) ) ;
#8468 = CARTESIAN_POINT ( 'NONE',  ( -15.79547310275335725, -3.553268508742920773, -224.0225025563328813 ) ) ;
#8469 = ORIENTED_EDGE ( 'NONE', *, *, #12730, .T. ) ;
#8470 = CARTESIAN_POINT ( 'NONE',  ( 9.107417252317809186, 16.30291009569977234, -218.0131178633739921 ) ) ;
#8471 = CARTESIAN_POINT ( 'NONE',  ( -16.66929017373293931, 3.065794289431343689, -220.7800282905443794 ) ) ;
#8472 = CARTESIAN_POINT ( 'NONE',  ( -17.65933056022148762, 0.7424667221540405260, -229.0964312085266386 ) ) ;
#8473 = EDGE_CURVE ( 'NONE', #10297, #4083, #19645, .T. ) ;
#8474 = CIRCLE ( 'NONE', #1271, 19.80000000000007887 ) ;
#8475 = CIRCLE ( 'NONE', #16018, 21.00000000000000000 ) ;
#8476 = DIRECTION ( 'NONE',  ( -2.162300680179923768E-16, -1.000000000000000000, 0.000000000000000000 ) ) ;
#8477 = CARTESIAN_POINT ( 'NONE',  ( 12.98364502352995942, 13.67380631913144029, -233.1535077318696096 ) ) ;
#8478 = CARTESIAN_POINT ( 'NONE',  ( -24.82235633397527508, 10.76243500821901300, -227.9886044494091948 ) ) ;
#8479 = CARTESIAN_POINT ( 'NONE',  ( -0.7286890422672397394, 21.00519367000705273, -234.2149015821977969 ) ) ;
#8480 = CARTESIAN_POINT ( 'NONE',  ( 21.92281339924938877, 16.67475415235398017, -231.9828670874568957 ) ) ;
#8481 = CARTESIAN_POINT ( 'NONE',  ( -14.91192530170583197, -15.94630704366669782, -215.1411503333790165 ) ) ;
#8482 = ORIENTED_EDGE ( 'NONE', *, *, #4601, .T. ) ;
#8483 = CARTESIAN_POINT ( 'NONE',  ( -5.534391910549205207, -14.54353160188980709, -228.1022699408985943 ) ) ;
#8484 = CARTESIAN_POINT ( 'NONE',  ( -23.66836017558062011, 21.44695383684080525, -223.6245772351065568 ) ) ;
#8485 = CARTESIAN_POINT ( 'NONE',  ( 1.904360901363437275, -12.77109371939166138, -224.5066922355585177 ) ) ;
#8486 = CARTESIAN_POINT ( 'NONE',  ( -8.172572110426221670, 16.86653848210977813, -233.4220330256369493 ) ) ;
#8487 = CARTESIAN_POINT ( 'NONE',  ( 28.08871713846552254, -6.057249427443905709, -231.1189077393881348 ) ) ;
#8488 = EDGE_CURVE ( 'NONE', #5604, #5555, #7314, .T. ) ;
#8489 = CARTESIAN_POINT ( 'NONE',  ( -16.39524763169126942, -10.97410814576847926, -232.9630882351523837 ) ) ;
#8490 = CARTESIAN_POINT ( 'NONE',  ( 10.25308675723727347, 13.16459519580956972, -229.3963488176951273 ) ) ;
#8491 = DIRECTION ( 'NONE',  ( -1.000000000000000000, 1.224646799147352961E-16, 0.000000000000000000 ) ) ;
#8492 = CARTESIAN_POINT ( 'NONE',  ( -8.221702953833418093, 11.87876791566348800, -223.9138461338794741 ) ) ;
#8493 = CARTESIAN_POINT ( 'NONE',  ( 15.74259730902452858, 17.40808440793174583, -232.1327802909178786 ) ) ;
#8494 = CARTESIAN_POINT ( 'NONE',  ( 22.86997486125673618, 17.56009411325475966, -222.3578648042903296 ) ) ;
#8495 = CARTESIAN_POINT ( 'NONE',  ( 14.96080648943632241, 22.28365808184747721, -220.1237743409445216 ) ) ;
#8496 = CARTESIAN_POINT ( 'NONE',  ( -4.239735564391798661, -14.20018808486349116, -230.2489621771221380 ) ) ;
#8497 = CARTESIAN_POINT ( 'NONE',  ( -3.162425552858488143, 20.40327580806445695, -216.0004724541873316 ) ) ;
#8498 = CARTESIAN_POINT ( 'NONE',  ( 14.80394259695730064, 1.224172658189580432, -225.4564070658925061 ) ) ;
#8499 = CARTESIAN_POINT ( 'NONE',  ( 8.082980660592431477, -16.66562551544545201, -231.4954396659114764 ) ) ;
#8500 = CARTESIAN_POINT ( 'NONE',  ( -16.28025842329327944, 6.985656672962045732, -231.4191468057695715 ) ) ;
#8501 = CIRCLE ( 'NONE', #5963, 23.00000000000000000 ) ;
#8502 = CARTESIAN_POINT ( 'NONE',  ( 3.378648530876271039, 26.08525450992624428, -218.4319906442508454 ) ) ;
#8503 =( GEOMETRIC_REPRESENTATION_CONTEXT ( 3 ) GLOBAL_UNCERTAINTY_ASSIGNED_CONTEXT ( ( #8085 ) ) GLOBAL_UNIT_ASSIGNED_CONTEXT ( ( #5060, #1469, #11937 ) ) REPRESENTATION_CONTEXT ( 'NONE', 'WORKASPACE' ) );
#8504 = CARTESIAN_POINT ( 'NONE',  ( -13.21314811618155716, -9.038438575223175064, -230.6430079410957603 ) ) ;
#8505 = CARTESIAN_POINT ( 'NONE',  ( 21.96352831578506937, -0.3315607655626218175, -233.9427286327412787 ) ) ;
#8506 = CARTESIAN_POINT ( 'NONE',  ( 7.393167209263542539, 10.77319710117329699, -221.1179833906701049 ) ) ;
#8507 = ORIENTED_EDGE ( 'NONE', *, *, #21758, .F. ) ;
#8508 = CARTESIAN_POINT ( 'NONE',  ( 4.343013938751969505, 13.02036404005131587, -224.7825435359082178 ) ) ;
#8509 = CARTESIAN_POINT ( 'NONE',  ( 13.96414008557630559, -4.972932825000588863, -226.4793371398648389 ) ) ;
#8510 = CARTESIAN_POINT ( 'NONE',  ( 22.46263922039936745, -3.404486942579552089, -216.1438077301478415 ) ) ;
#8511 = PRODUCT_DEFINITION_FORMATION_WITH_SPECIFIED_SOURCE ( 'ANY', '', #17154, .NOT_KNOWN. ) ;
#8512 = CARTESIAN_POINT ( 'NONE',  ( -3.514547081416551588, 30.38636916157537016, -227.3529586180979436 ) ) ;
#8513 = CARTESIAN_POINT ( 'NONE',  ( -18.68851093906118521, -8.564152624513159395, -215.1804141040323941 ) ) ;
#8514 = CARTESIAN_POINT ( 'NONE',  ( -0.6367083786117293531, -29.73461014436635708, -220.1383336929387724 ) ) ;
#8515 = CARTESIAN_POINT ( 'NONE',  ( 10.99893791904045415, -12.61823049403341201, -218.3266956685045841 ) ) ;
#8516 = CARTESIAN_POINT ( 'NONE',  ( -8.115738378024497379, 16.90402287339461296, -219.0833473190803034 ) ) ;
#8517 = CARTESIAN_POINT ( 'NONE',  ( 10.63406535173453271, 22.16595115341124256, -219.6461356279925781 ) ) ;
#8518 = CARTESIAN_POINT ( 'NONE',  ( -11.67631226053870996, 6.737291529340801333, -227.3110382950315227 ) ) ;
#8519 = CARTESIAN_POINT ( 'NONE',  ( -11.83206531956964902, 10.60028422373495260, -231.1115289952381033 ) ) ;
#8520 = CARTESIAN_POINT ( 'NONE',  ( -11.98587399847077783, -10.70615994290841044, -225.3229167341726225 ) ) ;
#8521 = CARTESIAN_POINT ( 'NONE',  ( -11.48592899399814726, 13.65854631785387774, -230.8311022452805616 ) ) ;
#8522 = CARTESIAN_POINT ( 'NONE',  ( 22.42925200799500729, 5.652256920629083581, -234.0734181799116698 ) ) ;
#8523 = CARTESIAN_POINT ( 'NONE',  ( 19.13589083395335422, 16.69125564174534659, -234.7442498487877174 ) ) ;
#8524 = CARTESIAN_POINT ( 'NONE',  ( 21.85730963248023428, -9.423385237436111339, -216.6089804361807580 ) ) ;
#8525 = DIRECTION ( 'NONE',  ( 0.000000000000000000, 0.000000000000000000, -1.000000000000000000 ) ) ;
#8526 = VERTEX_POINT ( 'NONE', #9317 ) ;
#8527 = CARTESIAN_POINT ( 'NONE',  ( -11.02345917017863464, 29.02019856777526741, -223.9475008740665771 ) ) ;
#8528 = CARTESIAN_POINT ( 'NONE',  ( -21.73784594492672895, -5.247588939251936146, -214.6321000900504714 ) ) ;
#8529 = FACE_OUTER_BOUND ( 'NONE', #17309, .T. ) ;
#8530 = CARTESIAN_POINT ( 'NONE',  ( 14.63113973005795643, 4.926264598692385199, -222.4866305912601945 ) ) ;
#8531 = CARTESIAN_POINT ( 'NONE',  ( -20.43618815875133521, 1.403378831510147196, -232.9646741665398224 ) ) ;
#8532 = CARTESIAN_POINT ( 'NONE',  ( 13.62757736989142465, -5.584028114184929947, -227.2616851496390211 ) ) ;
#8533 = CARTESIAN_POINT ( 'NONE',  ( -27.29953305526601426, 11.21644211419729054, -229.3676346105362995 ) ) ;
#8534 = PRODUCT_DEFINITION_SHAPE ( 'NONE', 'NONE',  #5050 ) ;
#8535 = CARTESIAN_POINT ( 'NONE',  ( 14.64440749032966593, 2.523901497798496596, -225.4572725674553340 ) ) ;
#8536 = CARTESIAN_POINT ( 'NONE',  ( -5.056986327342952947, -15.36481113542577503, -220.7955371552936583 ) ) ;
#8537 = CARTESIAN_POINT ( 'NONE',  ( 0.000000000000000000, 0.000000000000000000, -24.99999999999999645 ) ) ;
#8538 = CARTESIAN_POINT ( 'NONE',  ( 15.76910524310159900, 5.601482066865847820, -220.3440822020379528 ) ) ;
#8539 = CARTESIAN_POINT ( 'NONE',  ( -14.87984907657228639, 0.2138881189739126887, -228.7773920408832282 ) ) ;
#8540 = CARTESIAN_POINT ( 'NONE',  ( 14.99967020447171784, -24.16696097797641940, -221.8072564961694297 ) ) ;
#8541 = CARTESIAN_POINT ( 'NONE',  ( 12.80949378899885893, -2.780008750929118033, -226.1439410239644303 ) ) ;
#8542 = EDGE_CURVE ( 'NONE', #14013, #9212, #19535, .T. ) ;
#8543 = CARTESIAN_POINT ( 'NONE',  ( -20.74454492543941342, -9.934009332729857533, -1.323381102396829379 ) ) ;
#8544 = CARTESIAN_POINT ( 'NONE',  ( 7.497537106193371770, 19.52448593130572618, -231.1338690134634248 ) ) ;
#8545 = CARTESIAN_POINT ( 'NONE',  ( 8.856360819293511710, 14.24139612884802553, -227.7731680686805475 ) ) ;
#8546 = CARTESIAN_POINT ( 'NONE',  ( 6.498966860804143764, -11.65341448970024274, -221.3944939044252749 ) ) ;
#8547 = CARTESIAN_POINT ( 'NONE',  ( 8.709470447750865318, -17.43408031369701661, -216.5121658579468829 ) ) ;
#8548 = VERTEX_POINT ( 'NONE', #12360 ) ;
#8549 = CARTESIAN_POINT ( 'NONE',  ( -19.65084584916038324, 18.01805631773661176, -219.5040736310571106 ) ) ;
#8550 = CARTESIAN_POINT ( 'NONE',  ( -20.92673740658815973, 5.672885432599523270, -219.1433548642331459 ) ) ;
#8551 = CARTESIAN_POINT ( 'NONE',  ( 25.01541028746040141, 13.78427203520734423, -225.9266837950359843 ) ) ;
#8552 = VERTEX_POINT ( 'NONE', #7410 ) ;
#8553 = CARTESIAN_POINT ( 'NONE',  ( -7.536234698756538286, -25.83616497442384130, -229.4709156672317363 ) ) ;
#8554 = CARTESIAN_POINT ( 'NONE',  ( 5.709328484389686764, -9.211115167980509000, 91.99999999999998579 ) ) ;
#8555 = ORIENTED_EDGE ( 'NONE', *, *, #15991, .F. ) ;
#8556 = CARTESIAN_POINT ( 'NONE',  ( 14.68015846516680867, 2.651775288685355836, -224.1317433549420173 ) ) ;
#8557 = CARTESIAN_POINT ( 'NONE',  ( 9.672299229151310129, -14.28303711772943529, -228.3078296064027484 ) ) ;
#8558 = CARTESIAN_POINT ( 'NONE',  ( 7.762960416026701616, 12.60702317161859121, -221.9096828323375235 ) ) ;
#8559 = CARTESIAN_POINT ( 'NONE',  ( -18.70100282803782576, 16.58357028540773115, -216.4425743468854080 ) ) ;
#8560 = CARTESIAN_POINT ( 'NONE',  ( 5.773563157792669820, 21.63217468058455140, -235.0383461317610170 ) ) ;
#8561 = CARTESIAN_POINT ( 'NONE',  ( -12.98662328632235585, 28.83726371277012035, -223.5970274767108776 ) ) ;
#8562 = CARTESIAN_POINT ( 'NONE',  ( -11.42613629117093765, 28.09170287990588832, -228.7150250545069241 ) ) ;
#8563 = CARTESIAN_POINT ( 'NONE',  ( 8.059654651175295115, 7.153714881707382567, 92.00000000000001421 ) ) ;
#8564 = CARTESIAN_POINT ( 'NONE',  ( 5.982950994121768673, -14.58086824529316594, -231.1438280359330975 ) ) ;
#8565 = CARTESIAN_POINT ( 'NONE',  ( 28.78651053433536333, -0.9604905981993369091, -227.3547688931310233 ) ) ;
#8566 = LINE ( 'NONE', #3479, #12062 ) ;
#8567 = CARTESIAN_POINT ( 'NONE',  ( -28.18501077041064562, -8.523171531337160545, -227.0531053546762337 ) ) ;
#8568 = CARTESIAN_POINT ( 'NONE',  ( 24.03642272140365677, 3.646960756862087205, -218.2320643939070806 ) ) ;
#8569 = CARTESIAN_POINT ( 'NONE',  ( -19.84632485794307399, -12.65249528142034485, -231.0223831579344278 ) ) ;
#8570 = CARTESIAN_POINT ( 'NONE',  ( 6.025688374458400887, -15.61258154445926749, -220.0079782759978002 ) ) ;
#8571 = CARTESIAN_POINT ( 'NONE',  ( -28.31595744342370580, 5.786754998807587924, -229.0820962600229223 ) ) ;
#8572 = CARTESIAN_POINT ( 'NONE',  ( 10.03842945413050458, 28.43460431997513638, -225.8374938385031214 ) ) ;
#8573 = CARTESIAN_POINT ( 'NONE',  ( -6.072587425033909803, 24.65158735603439055, -217.4249768037189767 ) ) ;
#8574 = ORIENTED_EDGE ( 'NONE', *, *, #6806, .F. ) ;
#8575 = CARTESIAN_POINT ( 'NONE',  ( -17.04360437375341419, -3.174793268193519591, -228.4680687138289841 ) ) ;
#8576 = ORIENTED_EDGE ( 'NONE', *, *, #1423, .F. ) ;
#8577 = CARTESIAN_POINT ( 'NONE',  ( 22.46220731426537043, 18.23201731183003460, -227.5436199598787539 ) ) ;
#8578 = ADVANCED_FACE ( 'NONE', ( #15849 ), #11110, .T. ) ;
#8579 = CARTESIAN_POINT ( 'NONE',  ( -17.89085717681497201, 10.08962028281416856, -232.3705156551908431 ) ) ;
#8580 = CARTESIAN_POINT ( 'NONE',  ( -17.91550223652134122, 4.809113705933536487, -230.6324822114035555 ) ) ;
#8581 = CARTESIAN_POINT ( 'NONE',  ( -10.30161254035895091, -9.966167094494833734, -223.3409979381218875 ) ) ;
#8582 = AXIS2_PLACEMENT_3D ( 'NONE', #21784, #18861, #10317 ) ;
#8583 = CARTESIAN_POINT ( 'NONE',  ( 0.000000000000000000, 23.00000000000000000, -69.99999999999998579 ) ) ;
#8584 = CARTESIAN_POINT ( 'NONE',  ( 17.66525298603349370, 4.919957226727790456, -233.3736646485340032 ) ) ;
#8585 = CARTESIAN_POINT ( 'NONE',  ( -18.42638600874552424, 7.060399206045774534, -230.3991437614443214 ) ) ;
#8586 = CARTESIAN_POINT ( 'NONE',  ( 19.49137065790598555, 9.165486118354671419, -234.8706749352814995 ) ) ;
#8587 = EDGE_CURVE ( 'NONE', #18055, #9712, #7300, .T. ) ;
#8588 = CARTESIAN_POINT ( 'NONE',  ( 15.90795275983908574, 2.546196724714939297, -229.0855319561646297 ) ) ;
#8589 = CARTESIAN_POINT ( 'NONE',  ( -10.66474234094022755, -20.68992156881482813, -215.8674331684499634 ) ) ;
#8590 = VERTEX_POINT ( 'NONE', #14170 ) ;
#8591 = CARTESIAN_POINT ( 'NONE',  ( -10.06927776881013514, -17.00317020600589402, -217.8513858272130790 ) ) ;
#8592 = CARTESIAN_POINT ( 'NONE',  ( -9.964021556040458805, 12.25789996591640119, -217.8262340283327774 ) ) ;
#8593 = CARTESIAN_POINT ( 'NONE',  ( 2.967317674205219191, -16.40215926535219282, -217.6245344443522924 ) ) ;
#8594 = CARTESIAN_POINT ( 'NONE',  ( 1.217121169770782663, 15.31158828575123110, -230.6845728599757308 ) ) ;
#8595 = CARTESIAN_POINT ( 'NONE',  ( 11.58852274881379962, -8.803378160360782800, -231.6724139265004965 ) ) ;
#8596 = CARTESIAN_POINT ( 'NONE',  ( -25.82802808205240552, -14.78441951539553401, -222.6940535085979604 ) ) ;
#8597 = CARTESIAN_POINT ( 'NONE',  ( -13.81390866287826746, 1.832988708064121175, -224.4361041349432639 ) ) ;
#8598 = FACE_OUTER_BOUND ( 'NONE', #19239, .T. ) ;
#8599 = CARTESIAN_POINT ( 'NONE',  ( -2.806347010929339802, 19.90767250424812573, -230.9206976900916004 ) ) ;
#8600 = CARTESIAN_POINT ( 'NONE',  ( 17.41909632439413969, 2.006477695503792624, -233.4081875040758121 ) ) ;
#8601 = CARTESIAN_POINT ( 'NONE',  ( 15.87442104186276381, 8.674488492264579520, -230.9702037640878416 ) ) ;
#8602 = CARTESIAN_POINT ( 'NONE',  ( 16.48801037644500056, 3.165716804515234628, -216.8169430726136113 ) ) ;
#8603 = CARTESIAN_POINT ( 'NONE',  ( 4.579865149819754677, -13.09122092233156387, -219.1296897471712839 ) ) ;
#8604 = CARTESIAN_POINT ( 'NONE',  ( 12.58033168766476528, 20.35631482982274676, -235.1670639654690547 ) ) ;
#8605 = CARTESIAN_POINT ( 'NONE',  ( 17.07668571305246985, 2.037405138410691485, -219.7626854147787867 ) ) ;
#8606 = CARTESIAN_POINT ( 'NONE',  ( 12.13370821170821223, -20.35915274155448174, -217.8532457648388458 ) ) ;
#8607 = CARTESIAN_POINT ( 'NONE',  ( -21.19360951076126653, 12.15251088906093457, -217.9482185194656552 ) ) ;
#8608 = CARTESIAN_POINT ( 'NONE',  ( 8.175342817246784577, 19.41817470142738244, -216.6818271833384699 ) ) ;
#8609 = CARTESIAN_POINT ( 'NONE',  ( -11.88525712185471050, -8.925198460467992589, -221.0951487055306472 ) ) ;
#8610 = CARTESIAN_POINT ( 'NONE',  ( 24.81079154715000357, 3.171651085595392772, -216.4177249688571578 ) ) ;
#8611 = ADVANCED_FACE ( 'NONE', ( #5595 ), #17350, .F. ) ;
#8612 = CARTESIAN_POINT ( 'NONE',  ( 17.88619020626327938, 19.43517936004721847, -216.7078103882350604 ) ) ;
#8613 = CARTESIAN_POINT ( 'NONE',  ( 13.61707622192329481, 14.84143455326118932, -217.6958999636067063 ) ) ;
#8614 = CARTESIAN_POINT ( 'NONE',  ( 13.49585564903807722, -8.492623513249517586, -227.3331091713134811 ) ) ;
#8615 = CARTESIAN_POINT ( 'NONE',  ( 25.90657540470570197, -10.31326923046670885, -218.6707845005603019 ) ) ;
#8616 = LINE ( 'NONE', #390, #18148 ) ;
#8617 = CARTESIAN_POINT ( 'NONE',  ( 18.50911814746675788, 15.92944434255054453, -232.0449215596906072 ) ) ;
#8618 = CARTESIAN_POINT ( 'NONE',  ( -11.84714279977019125, -8.528511525072332233, -232.0239825124074002 ) ) ;
#8619 = CARTESIAN_POINT ( 'NONE',  ( -8.379125946468517938, -29.31735857037017468, -221.8060643354269814 ) ) ;
#8620 = CARTESIAN_POINT ( 'NONE',  ( 5.434900225474387447, -11.93567727083262042, -224.7511004068755369 ) ) ;
#8621 = CARTESIAN_POINT ( 'NONE',  ( -2.993956627714193353, 22.04778837082692178, -231.1741803919495339 ) ) ;
#8622 = CARTESIAN_POINT ( 'NONE',  ( 28.52435124311170966, 7.611291969169514005, -224.8315247833735384 ) ) ;
#8623 = CARTESIAN_POINT ( 'NONE',  ( -22.47200958260654957, 4.697452857301940732, -216.5879371680706242 ) ) ;
#8624 = CARTESIAN_POINT ( 'NONE',  ( -8.752190949579933488, 24.25633523490762755, -230.6624101830059885 ) ) ;
#8625 = CARTESIAN_POINT ( 'NONE',  ( 17.44158214791148964, -8.186237638883257617, -216.9355394212118995 ) ) ;
#8626 = ORIENTED_EDGE ( 'NONE', *, *, #7604, .T. ) ;
#8627 = CARTESIAN_POINT ( 'NONE',  ( -16.57767831947938575, 23.50485984366324388, -222.7977068309636763 ) ) ;
#8628 = CARTESIAN_POINT ( 'NONE',  ( 29.55842656951424985, 4.785221541509360854, -220.5134865854112718 ) ) ;
#8629 = CARTESIAN_POINT ( 'NONE',  ( 18.65058977333779211, 24.40868228550881014, -219.3406275662563303 ) ) ;
#8630 = CARTESIAN_POINT ( 'NONE',  ( 12.12535264607833341, -6.902938132833007501, -227.3565233277489597 ) ) ;
#8631 = CARTESIAN_POINT ( 'NONE',  ( 13.55929460187270053, 0.3562519042583365270, -227.9787723277739246 ) ) ;
#8632 = ORIENTED_EDGE ( 'NONE', *, *, #14777, .F. ) ;
#8633 = CARTESIAN_POINT ( 'NONE',  ( -0.1571923090946999446, 19.34188126963334398, -216.6893131123363787 ) ) ;
#8634 = CARTESIAN_POINT ( 'NONE',  ( -8.763358281418030415, -9.103836352148345412, -222.0692104753270257 ) ) ;
#8635 = CARTESIAN_POINT ( 'NONE',  ( 26.00000000000000000, -0.5000000000000000000, 0.000000000000000000 ) ) ;
#8636 = CARTESIAN_POINT ( 'NONE',  ( 21.35706335192880445, 15.67286272432725092, -219.2578158352350783 ) ) ;
#8637 = CARTESIAN_POINT ( 'NONE',  ( -14.10849459794400751, -0.2436790717799666162, -223.1085195285415921 ) ) ;
#8638 = CARTESIAN_POINT ( 'NONE',  ( 15.11994912051959972, -12.48385213956034079, -232.8079920308188377 ) ) ;
#8639 = CARTESIAN_POINT ( 'NONE',  ( -17.84981083811007707, 0.8485253248287054628, -231.8041300026935119 ) ) ;
#8640 = CARTESIAN_POINT ( 'NONE',  ( -15.20262116893801974, 8.038155052917188570, -217.6767387945475036 ) ) ;
#8641 = CARTESIAN_POINT ( 'NONE',  ( -3.176860551132370425, -19.01962362838126452, -231.5826211182368297 ) ) ;
#8642 = FACE_OUTER_BOUND ( 'NONE', #16446, .T. ) ;
#8643 = CARTESIAN_POINT ( 'NONE',  ( -21.73559549195910634, 7.536301886650155879, 6.604919831454106216 ) ) ;
#8644 = CARTESIAN_POINT ( 'NONE',  ( -13.56774755469388616, 7.311522441667196226, -219.1912666243428021 ) ) ;
#8645 = CARTESIAN_POINT ( 'NONE',  ( 19.65870185572374140, -17.77243814521307641, -229.4329728153015253 ) ) ;
#8646 = CARTESIAN_POINT ( 'NONE',  ( 13.24751142555096273, -1.959735780492239288, -222.7273387214888203 ) ) ;
#8647 = CARTESIAN_POINT ( 'NONE',  ( -24.79589088527667684, 3.246309046422540590, 9.481087457883008440 ) ) ;
#8648 = CARTESIAN_POINT ( 'NONE',  ( 16.53859560591101641, 22.24348416270211359, -223.7250258089275974 ) ) ;
#8649 = CARTESIAN_POINT ( 'NONE',  ( 5.585286719045844173, 27.51657303716567426, -222.4190945945824751 ) ) ;
#8650 = CARTESIAN_POINT ( 'NONE',  ( 3.436191426816104233, -15.97976940388950773, -231.4631329546418499 ) ) ;
#8651 = CARTESIAN_POINT ( 'NONE',  ( 8.785770181087007913, -10.38731345016515917, -223.4272116603623317 ) ) ;
#8652 = ORIENTED_EDGE ( 'NONE', *, *, #12559, .T. ) ;
#8653 = CARTESIAN_POINT ( 'NONE',  ( -10.30870167223346456, 11.95603877111467561, -228.4123369090513336 ) ) ;
#8654 = CARTESIAN_POINT ( 'NONE',  ( -24.40185606299549192, 11.66496215664722236, -221.9473669705449765 ) ) ;
#8655 = CARTESIAN_POINT ( 'NONE',  ( -12.12559971566433958, 1.856299769312002912, -227.8748781050665286 ) ) ;
#8656 = CARTESIAN_POINT ( 'NONE',  ( -11.97657177269377371, -18.30092786828533846, -219.1278344157730942 ) ) ;
#8657 = DIRECTION ( 'NONE',  ( 1.000000000000000000, 0.000000000000000000, 0.000000000000000000 ) ) ;
#8658 = ORIENTED_EDGE ( 'NONE', *, *, #21602, .T. ) ;
#8659 = CARTESIAN_POINT ( 'NONE',  ( 23.64727379217503866, 9.907944788639682088, -232.0643337313508709 ) ) ;
#8660 = CARTESIAN_POINT ( 'NONE',  ( 9.097575839043912538, -18.13002900832716335, -219.2719510042808224 ) ) ;
#8661 = CARTESIAN_POINT ( 'NONE',  ( 17.68508104102419409, 23.41266195669770767, -227.5327139115408954 ) ) ;
#8662 = CARTESIAN_POINT ( 'NONE',  ( -8.966714183099560032, 19.05224306381768073, -234.0879867025980445 ) ) ;
#8663 = ADVANCED_FACE ( 'NONE', ( #12688 ), #469, .F. ) ;
#8664 = CARTESIAN_POINT ( 'NONE',  ( 25.30941179858102430, 8.661697827793627624, -216.7530520919057722 ) ) ;
#8665 = CARTESIAN_POINT ( 'NONE',  ( 5.248230734842167955, 23.54336384919183445, -216.8914391693808739 ) ) ;
#8666 = CARTESIAN_POINT ( 'NONE',  ( 10.76794919243112680, 1.500192839452123339, 91.99999999999997158 ) ) ;
#8667 = CARTESIAN_POINT ( 'NONE',  ( -1.778254167844783851, -12.78790610364390012, -225.9413532495922254 ) ) ;
#8668 = CARTESIAN_POINT ( 'NONE',  ( 13.38839277810360429, -5.174145297632733786, -223.8523798909600941 ) ) ;
#8669 = DIRECTION ( 'NONE',  ( -0.000000000000000000, 0.000000000000000000, -1.000000000000000000 ) ) ;
#8670 = CARTESIAN_POINT ( 'NONE',  ( 1.526556658859590243E-13, -21.80000000000000071, -78.50000000000000000 ) ) ;
#8671 = CARTESIAN_POINT ( 'NONE',  ( 20.58703255433590940, 0.4816031003617209372, -231.9427175861361263 ) ) ;
#8672 = CARTESIAN_POINT ( 'NONE',  ( -13.33153391309230074, -13.53657406488594184, -231.3594229707590557 ) ) ;
#8673 = CARTESIAN_POINT ( 'NONE',  ( 9.835929410207317147, -16.71508016877321268, -232.2716196330763694 ) ) ;
#8674 = CARTESIAN_POINT ( 'NONE',  ( 26.06405806384012536, 5.488112530166501024, -216.5020692413490622 ) ) ;
#8675 = CARTESIAN_POINT ( 'NONE',  ( -1.975202609796049336, 20.81351768191813889, -217.5779402428482001 ) ) ;
#8676 = CARTESIAN_POINT ( 'NONE',  ( -1.386728072030569692, 16.52832439466973824, -230.7516952943509807 ) ) ;
#8677 = ORIENTED_EDGE ( 'NONE', *, *, #12559, .F. ) ;
#8678 = CARTESIAN_POINT ( 'NONE',  ( 29.53814377227115884, -10.02285884041311270, -220.1614914916521286 ) ) ;
#8679 = VERTEX_POINT ( 'NONE', #2211 ) ;
#8680 = CARTESIAN_POINT ( 'NONE',  ( 8.979547488457603421, 23.24376652602565230, -232.6628827740196357 ) ) ;
#8681 = CARTESIAN_POINT ( 'NONE',  ( -19.61183938075907918, 22.25855138946451106, -229.5731876748794207 ) ) ;
#8682 = CARTESIAN_POINT ( 'NONE',  ( -15.82952867276381603, 3.677461268355039170, -227.9997968350711801 ) ) ;
#8683 = CARTESIAN_POINT ( 'NONE',  ( -7.972347216402701164, -18.74702622849856937, -232.1058264431568148 ) ) ;
#8684 = CARTESIAN_POINT ( 'NONE',  ( 0.000000000000000000, 21.00000000000006040, 69.99999999999998579 ) ) ;
#8685 = CARTESIAN_POINT ( 'NONE',  ( 14.00715608756928532, 4.299235856235253728, -230.2440235370780215 ) ) ;
#8686 = CARTESIAN_POINT ( 'NONE',  ( -16.48883219358909713, 20.84100960965193394, -219.4392138569792507 ) ) ;
#8687 = CARTESIAN_POINT ( 'NONE',  ( 12.08790845148079640, 6.355304031620478078, -220.0087475230167229 ) ) ;
#8688 = CARTESIAN_POINT ( 'NONE',  ( 12.91815243135930480, 5.607966342865584153, -224.2227256053222959 ) ) ;
#8689 = EDGE_CURVE ( 'NONE', #16045, #11119, #2956, .T. ) ;
#8690 = CARTESIAN_POINT ( 'NONE',  ( -13.61368873860109652, -1.873405602088730859, -231.0542245685610112 ) ) ;
#8691 = ORIENTED_EDGE ( 'NONE', *, *, #21072, .T. ) ;
#8692 = CARTESIAN_POINT ( 'NONE',  ( -13.29422863469367577, -26.11207831950312652, -226.3284374130324750 ) ) ;
#8693 = CARTESIAN_POINT ( 'NONE',  ( -21.50655177804914686, 20.61731362457859973, -218.7935603611527426 ) ) ;
#8694 = CARTESIAN_POINT ( 'NONE',  ( 7.437838793555467731, -20.85539581353325289, -233.9154700400843865 ) ) ;
#8695 = CARTESIAN_POINT ( 'NONE',  ( 2.539761864897490007, 23.64215977235053501, -233.4645566207487661 ) ) ;
#8696 = CARTESIAN_POINT ( 'NONE',  ( 17.11616244378571494, -1.720737510755655064, -232.0394440302203236 ) ) ;
#8697 = CARTESIAN_POINT ( 'NONE',  ( -22.05223281125454804, 0.4748437386657365367, -217.8785187290425256 ) ) ;
#8698 = CARTESIAN_POINT ( 'NONE',  ( 13.06430160593375689, 2.561628050526134182, -220.6026188403641299 ) ) ;
#8699 = CARTESIAN_POINT ( 'NONE',  ( -8.791002657293931932, 17.82034842365333205, -218.5247019341474584 ) ) ;
#8700 = CARTESIAN_POINT ( 'NONE',  ( 17.23039831256031817, 3.331158952577910615, -216.4027685342793461 ) ) ;
#8701 = CIRCLE ( 'NONE', #18401, 3.000000000000002665 ) ;
#8702 = CARTESIAN_POINT ( 'NONE',  ( 10.57926812561479757, 10.00910231482511215, -225.8341706491384286 ) ) ;
#8703 = CARTESIAN_POINT ( 'NONE',  ( 13.17768061945195157, 6.810183613937965674, -219.8302315341053657 ) ) ;
#8704 = CARTESIAN_POINT ( 'NONE',  ( -0.1874296312810625753, -16.87674362306512776, -233.1597105263269611 ) ) ;
#8705 = CARTESIAN_POINT ( 'NONE',  ( 7.359401564398577733, 15.81697286067417707, -215.8326977948377987 ) ) ;
#8706 = AXIS2_PLACEMENT_3D ( 'NONE', #9191, #10763, #17628 ) ;
#8707 = CARTESIAN_POINT ( 'NONE',  ( 22.18132842682159733, 5.591149267797686839, -232.0584733989884114 ) ) ;
#8708 = CARTESIAN_POINT ( 'NONE',  ( 1.780865994697476307, -30.77012162006053941, -222.8552464324424705 ) ) ;
#8709 = CARTESIAN_POINT ( 'NONE',  ( -7.873497077133136735, 15.44270125396616677, -230.2562282217168672 ) ) ;
#8710 = CARTESIAN_POINT ( 'NONE',  ( 12.08198696763335178, 15.54678077493410981, -216.6084679670902631 ) ) ;
#8711 = CIRCLE ( 'NONE', #14838, 13.12488928717151637 ) ;
#8712 = CARTESIAN_POINT ( 'NONE',  ( -15.51091956967506391, -1.782849713491490018, -228.8089183834494520 ) ) ;
#8713 = CARTESIAN_POINT ( 'NONE',  ( -18.92390258637512090, 12.75887082072172163, -230.9970325548277970 ) ) ;
#8714 = CARTESIAN_POINT ( 'NONE',  ( -14.08236938285573636, 6.062428076406559008, -221.7923619418395447 ) ) ;
#8715 = CARTESIAN_POINT ( 'NONE',  ( 13.59483335902903178, 5.678732573479117640, -228.5032236586631313 ) ) ;
#8716 = ORIENTED_EDGE ( 'NONE', *, *, #2633, .F. ) ;
#8717 = CARTESIAN_POINT ( 'NONE',  ( 10.07175337281514871, 14.76776740066196325, -231.7834566702614723 ) ) ;
#8718 = CARTESIAN_POINT ( 'NONE',  ( 9.790069677392189362, -14.58761328102826837, -228.7245293813585647 ) ) ;
#8719 = VERTEX_POINT ( 'NONE', #642 ) ;
#8720 = CARTESIAN_POINT ( 'NONE',  ( 13.20312407767240614, -7.650902547765872086, -230.0578600405493717 ) ) ;
#8721 = CARTESIAN_POINT ( 'NONE',  ( -2.723069588102707606, 15.58614045890443833, -225.0254611642426141 ) ) ;
#8722 = EDGE_LOOP ( 'NONE', ( #7547, #13016, #10974, #3780 ) ) ;
#8723 = DIRECTION ( 'NONE',  ( -1.000000000000000000, 1.224646799147353454E-16, 0.000000000000000000 ) ) ;
#8724 = CARTESIAN_POINT ( 'NONE',  ( 12.71450444683213021, 7.595266944807587350, -224.4213778964231665 ) ) ;
#8725 = CARTESIAN_POINT ( 'NONE',  ( -9.442378551029269929, -6.949684989614740793, -225.4111852319283855 ) ) ;
#8726 = CARTESIAN_POINT ( 'NONE',  ( -6.642805165258356404, -28.12267032419628521, -230.9452027245340560 ) ) ;
#8727 = CARTESIAN_POINT ( 'NONE',  ( 10.24538335401965661, -11.82980241027587276, -219.3753974371782363 ) ) ;
#8728 = CARTESIAN_POINT ( 'NONE',  ( -2.554014161526931392, 17.56271496069470572, -229.4905841158208659 ) ) ;
#8729 = DIRECTION ( 'NONE',  ( 0.000000000000000000, -0.000000000000000000, 1.000000000000000000 ) ) ;
#8730 = CARTESIAN_POINT ( 'NONE',  ( 14.23294950300690331, 6.961167337017927892, -222.0879133937260974 ) ) ;
#8731 = CARTESIAN_POINT ( 'NONE',  ( -26.74045434827795020, 12.41518252455047744, -220.4617428697642652 ) ) ;
#8732 = CARTESIAN_POINT ( 'NONE',  ( -5.560972518124746244, 14.60655266358653215, -227.5460946431043681 ) ) ;
#8733 = CARTESIAN_POINT ( 'NONE',  ( 23.84888352507021736, -3.411310983279423947, -216.3556234003997645 ) ) ;
#8734 = AXIS2_PLACEMENT_3D ( 'NONE', #10949, #19378, #16020 ) ;
#8735 = CIRCLE ( 'NONE', #17733, 12.50000000000000355 ) ;
#8736 = CARTESIAN_POINT ( 'NONE',  ( 3.291078285693179950, 23.55624334554876498, -217.3208248278388623 ) ) ;
#8737 = CARTESIAN_POINT ( 'NONE',  ( -17.29038495093124084, 2.707785585324113065, -229.0475017805649998 ) ) ;
#8738 = CARTESIAN_POINT ( 'NONE',  ( 10.93653298376230687, 10.42959444671468106, -232.5920418140667039 ) ) ;
#8739 = EDGE_CURVE ( 'NONE', #1956, #1152, #2247, .T. ) ;
#8740 = CARTESIAN_POINT ( 'NONE',  ( 5.037691872308702301, -15.96383311541683270, -230.0422288358542460 ) ) ;
#8741 = CARTESIAN_POINT ( 'NONE',  ( 0.000000000000000000, -17.50000000000000711, -24.99999999999999645 ) ) ;
#8742 = VERTEX_POINT ( 'NONE', #12799 ) ;
#8743 = CARTESIAN_POINT ( 'NONE',  ( -3.326157069579807946, 13.92020081821418565, -220.5733722327383930 ) ) ;
#8744 = EDGE_CURVE ( 'NONE', #13719, #14896, #4398, .T. ) ;
#8745 = CARTESIAN_POINT ( 'NONE',  ( 27.74277644662361197, -2.671700443591659369, -227.2909148725441355 ) ) ;
#8746 = DIRECTION ( 'NONE',  ( 0.000000000000000000, 0.000000000000000000, -1.000000000000000000 ) ) ;
#8747 = CARTESIAN_POINT ( 'NONE',  ( 18.46552355142154411, 5.019711608606525211, -231.5099115070375433 ) ) ;
#8748 = ADVANCED_FACE ( 'NONE', ( #14713 ), #19752, .F. ) ;
#8749 = CARTESIAN_POINT ( 'NONE',  ( -13.93333636822611155, 3.327141996558931947, -221.4468162587888287 ) ) ;
#8750 = CARTESIAN_POINT ( 'NONE',  ( 11.31395536621571019, -8.070181239749643964, -225.0898076798974614 ) ) ;
#8751 =( NAMED_UNIT ( * ) PLANE_ANGLE_UNIT ( ) SI_UNIT ( $, .RADIAN. ) );
#8752 = CARTESIAN_POINT ( 'NONE',  ( -15.58461825850822180, 18.91734573546571951, -233.7691177939990723 ) ) ;
#8753 = CIRCLE ( 'NONE', #2973, 3.000000000000002665 ) ;
#8754 = CARTESIAN_POINT ( 'NONE',  ( -25.61997837663875188, 10.01664178086244483, -231.6711741719404074 ) ) ;
#8755 = CARTESIAN_POINT ( 'NONE',  ( -7.182761810198031505, -27.78193072152378207, -222.3754761716870973 ) ) ;
#8756 = VECTOR ( 'NONE', #14483, 1000.000000000000000 ) ;
#8757 = DIRECTION ( 'NONE',  ( -1.000000000000000000, 0.000000000000000000, 0.000000000000000000 ) ) ;
#8758 = CARTESIAN_POINT ( 'NONE',  ( 15.50884165284638705, 1.028647572718199843, -227.8181348745474679 ) ) ;
#8759 = CARTESIAN_POINT ( 'NONE',  ( -16.65698539163286540, 11.03290537638306112, -233.6474915129378758 ) ) ;
#8760 = CARTESIAN_POINT ( 'NONE',  ( 12.13370821170821223, -20.35915274155448174, -217.8532457648388458 ) ) ;
#8761 = CARTESIAN_POINT ( 'NONE',  ( 13.92874801379968730, -1.549146272830121518, -222.4308591964825439 ) ) ;
#8762 = CARTESIAN_POINT ( 'NONE',  ( -24.96744712291844337, 1.317343280566261265, 9.918382748296247442 ) ) ;
#8763 = CARTESIAN_POINT ( 'NONE',  ( 28.46362550855882745, 7.392895870364313282, -223.4682258299149566 ) ) ;
#8764 = CARTESIAN_POINT ( 'NONE',  ( -10.59650102373989533, 7.849913810122476576, -230.0486530042683171 ) ) ;
#8765 = CARTESIAN_POINT ( 'NONE',  ( 14.72648027392381387, 10.15511732729369676, -229.5776536674053716 ) ) ;
#8766 = CARTESIAN_POINT ( 'NONE',  ( -3.424870747449708652, -17.07003249573819659, -220.0803597572327135 ) ) ;
#8767 = CARTESIAN_POINT ( 'NONE',  ( 13.78060503451313323, -0.3076571220309521904, -222.4352540772387101 ) ) ;
#8768 = ORIENTED_EDGE ( 'NONE', *, *, #20103, .T. ) ;
#8769 = CARTESIAN_POINT ( 'NONE',  ( -1.975202609796049336, 20.81351768191813889, -217.5779402428482001 ) ) ;
#8770 = CARTESIAN_POINT ( 'NONE',  ( -13.91323058514953637, 8.006348396443080162, -225.5064972756604220 ) ) ;
#8771 = CARTESIAN_POINT ( 'NONE',  ( -22.10934047915441170, 0.9940043559354162506, -215.0000000000000000 ) ) ;
#8772 = ORIENTED_EDGE ( 'NONE', *, *, #5288, .T. ) ;
#8773 = CARTESIAN_POINT ( 'NONE',  ( -18.84435272498963343, -14.36455033211084498, -230.7675749430951555 ) ) ;
#8774 = CARTESIAN_POINT ( 'NONE',  ( -23.00000000000000000, 0.000000000000000000, -24.99999999999999645 ) ) ;
#8775 = VECTOR ( 'NONE', #11451, 1000.000000000000000 ) ;
#8776 = ORIENTED_EDGE ( 'NONE', *, *, #22191, .F. ) ;
#8777 = AXIS2_PLACEMENT_3D ( 'NONE', #2533, #19203, #7511 ) ;
#8778 = CARTESIAN_POINT ( 'NONE',  ( 24.81668481317358399, 17.11438712655213124, -222.1096362285750274 ) ) ;
#8779 = CARTESIAN_POINT ( 'NONE',  ( 18.69764316139794147, -20.69319383826335823, -224.5905439953889413 ) ) ;
#8780 = CARTESIAN_POINT ( 'NONE',  ( 3.449504654906655254, 27.59247159270940841, -231.3461799890608859 ) ) ;
#8781 = CARTESIAN_POINT ( 'NONE',  ( -9.250876228778270871, 9.538614635316015722, -227.1332118982684563 ) ) ;
#8782 = CARTESIAN_POINT ( 'NONE',  ( 11.17228388010293649, 5.622653638471959425, -222.3672781564363845 ) ) ;
#8783 = EDGE_CURVE ( 'NONE', #21666, #11033, #11954, .T. ) ;
#8784 = CARTESIAN_POINT ( 'NONE',  ( 10.02513374692848913, 18.81568788741115128, -217.1505009242214612 ) ) ;
#8785 = CARTESIAN_POINT ( 'NONE',  ( 0.000000000000000000, 0.000000000000000000, -30.00000000000000000 ) ) ;
#8786 = CARTESIAN_POINT ( 'NONE',  ( 5.451525948382545117, -12.45300865616632713, -227.8545162512558306 ) ) ;
#8787 = CARTESIAN_POINT ( 'NONE',  ( 13.91151814069282722, -15.58123622716646572, -216.5183035683795367 ) ) ;
#8788 = CARTESIAN_POINT ( 'NONE',  ( 0.000000000000000000, 0.000000000000000000, -24.99999999999999645 ) ) ;
#8789 = CIRCLE ( 'NONE', #18130, 17.50000000000000355 ) ;
#8790 = DIRECTION ( 'NONE',  ( 0.000000000000000000, 0.000000000000000000, 1.000000000000000000 ) ) ;
#8791 = CARTESIAN_POINT ( 'NONE',  ( -14.63872435137796302, 9.306825831109410530, -216.0000338566471214 ) ) ;
#8792 = CARTESIAN_POINT ( 'NONE',  ( -26.10238271615538252, -1.908654064438627174, -220.4792571320490708 ) ) ;
#8793 = CARTESIAN_POINT ( 'NONE',  ( 12.47670316482120967, 2.249148913447538423, -227.4574095259895898 ) ) ;
#8794 = CARTESIAN_POINT ( 'NONE',  ( 3.378648530876271039, 26.08525450992624428, -218.4319906442508454 ) ) ;
#8795 = CARTESIAN_POINT ( 'NONE',  ( 5.466128392039544259, 27.94759090250835243, -223.5617905851570981 ) ) ;
#8796 = VERTEX_POINT ( 'NONE', #11541 ) ;
#8797 = CARTESIAN_POINT ( 'NONE',  ( 26.96734317869073294, -1.796611605495658681, -216.2358245450472509 ) ) ;
#8798 = CARTESIAN_POINT ( 'NONE',  ( 21.53262694368047647, 11.06794636811408594, -231.8394491640143826 ) ) ;
#8799 = CARTESIAN_POINT ( 'NONE',  ( -12.26337789213896201, 9.274758280606999250, -219.9806108963443876 ) ) ;
#8800 = CARTESIAN_POINT ( 'NONE',  ( -19.58639255110637478, 14.91076398872931819, -217.1105532241463720 ) ) ;
#8801 = CARTESIAN_POINT ( 'NONE',  ( -11.55581979318669639, -19.97716813486601239, -217.5317483122086912 ) ) ;
#8802 = CARTESIAN_POINT ( 'NONE',  ( -28.17543631911187063, 3.557555778861649642, -230.1980773687482156 ) ) ;
#8803 = DIRECTION ( 'NONE',  ( 0.000000000000000000, 0.000000000000000000, -1.000000000000000000 ) ) ;
#8804 = DIRECTION ( 'NONE',  ( 1.000000000000000000, 0.000000000000000000, -0.000000000000000000 ) ) ;
#8805 = CARTESIAN_POINT ( 'NONE',  ( 13.54927135793711557, 0.6749664302445949060, -222.0769159577524192 ) ) ;
#8806 = CARTESIAN_POINT ( 'NONE',  ( -22.36207348798144778, 17.12313795477538036, -223.8571857210765472 ) ) ;
#8807 = CARTESIAN_POINT ( 'NONE',  ( 18.65058977333779211, 24.40868228550881014, -219.3406275662563303 ) ) ;
#8808 = CARTESIAN_POINT ( 'NONE',  ( -29.30406754532526037, 5.063969254119831120, -221.8212091093853076 ) ) ;
#8809 = CARTESIAN_POINT ( 'NONE',  ( -17.01570095888788003, -2.024181990473361115, -234.1256067144893791 ) ) ;
#8810 = ORIENTED_EDGE ( 'NONE', *, *, #15067, .T. ) ;
#8811 = CARTESIAN_POINT ( 'NONE',  ( -14.76610802599379291, -3.249507257478274180, -230.1617063156812719 ) ) ;
#8812 = CARTESIAN_POINT ( 'NONE',  ( -8.716816145717144693, 12.22834664005217675, -231.7124508691059646 ) ) ;
#8813 = CARTESIAN_POINT ( 'NONE',  ( -15.17658589853145479, -26.64966442869902252, -226.8090782225333442 ) ) ;
#8814 = CARTESIAN_POINT ( 'NONE',  ( 4.543450689403089271, 15.91052110650461771, -218.9437823786444426 ) ) ;
#8815 = CARTESIAN_POINT ( 'NONE',  ( 21.94513595990333954, -23.27941424421253203, -222.2428713697011631 ) ) ;
#8816 = DIRECTION ( 'NONE',  ( 0.000000000000000000, 0.000000000000000000, 1.000000000000000000 ) ) ;
#8817 = CARTESIAN_POINT ( 'NONE',  ( -29.16153046926437753, 6.356672163541281506, -226.4393515956758165 ) ) ;
#8818 = CARTESIAN_POINT ( 'NONE',  ( -7.928079932584687128, 26.12067226064367986, -221.2051195461628197 ) ) ;
#8819 = CARTESIAN_POINT ( 'NONE',  ( 12.15450584778660570, 2.288537795953278220, -225.7049340319972828 ) ) ;
#8820 = CARTESIAN_POINT ( 'NONE',  ( 15.76910524310159900, 5.601482066865847820, -220.3440822020379528 ) ) ;
#8821 = CARTESIAN_POINT ( 'NONE',  ( 12.47670316482120967, 2.249148913447538423, -227.4574095259895898 ) ) ;
#8822 = CARTESIAN_POINT ( 'NONE',  ( 0.4137397183702169468, -14.31347623323147289, -219.6167997211809393 ) ) ;
#8823 = CARTESIAN_POINT ( 'NONE',  ( 7.651502705057454889, 16.60422307457919544, -215.4679461133464144 ) ) ;
#8824 = CARTESIAN_POINT ( 'NONE',  ( 20.58703255433590940, 0.4816031003617209372, -231.9427175861361263 ) ) ;
#8825 = CARTESIAN_POINT ( 'NONE',  ( 0.8130732720878883768, -26.02312037787507393, -216.7203152272084878 ) ) ;
#8826 = CARTESIAN_POINT ( 'NONE',  ( -5.775873073292457249, 17.47547275616994256, -218.7209647771908578 ) ) ;
#8827 = CARTESIAN_POINT ( 'NONE',  ( 12.98364502352995942, 13.67380631913144029, -233.1535077318696096 ) ) ;
#8828 = CARTESIAN_POINT ( 'NONE',  ( -27.85133024402786006, -1.794102530182491773, -229.4204807338591081 ) ) ;
#8829 = CARTESIAN_POINT ( 'NONE',  ( -22.53796032816233463, 16.84148256071415872, -226.0516062466300582 ) ) ;
#8830 = CARTESIAN_POINT ( 'NONE',  ( -4.365576370787875859, 13.02741211227440665, -230.2897948137907917 ) ) ;
#8831 = CARTESIAN_POINT ( 'NONE',  ( 27.08994772491946890, 9.675875910685000747, -221.3471992134593336 ) ) ;
#8832 = VERTEX_POINT ( 'NONE', #6031 ) ;
#8833 = CARTESIAN_POINT ( 'NONE',  ( 6.900253619295916963, -14.54306101932516881, -223.7596260804713211 ) ) ;
#8834 = AXIS2_PLACEMENT_3D ( 'NONE', #22202, #7013, #12186 ) ;
#8835 = ORIENTED_EDGE ( 'NONE', *, *, #5705, .T. ) ;
#8836 = CARTESIAN_POINT ( 'NONE',  ( 19.78534257568999166, -22.00365353819481840, -227.2618024355658974 ) ) ;
#8837 = CARTESIAN_POINT ( 'NONE',  ( -5.600903697806950632, 21.62055466701630735, -218.6671277943675307 ) ) ;
#8838 = EDGE_LOOP ( 'NONE', ( #4205, #13568, #21735, #16900, #15673, #4993, #9825, #16082 ) ) ;
#8839 = DIRECTION ( 'NONE',  ( -1.000000000000000000, 0.000000000000000000, 0.000000000000000000 ) ) ;
#8840 = CARTESIAN_POINT ( 'NONE',  ( 7.762960416026701616, 12.60702317161859121, -221.9096828323375235 ) ) ;
#8841 = CARTESIAN_POINT ( 'NONE',  ( 22.03647168421188240, 0.3315607655626218175, -232.0572713672587213 ) ) ;
#8842 = CARTESIAN_POINT ( 'NONE',  ( -1.489322793389167288, -21.37773154815333498, -215.8826219457350817 ) ) ;
#8843 = CARTESIAN_POINT ( 'NONE',  ( -1.632242579688942596, -13.62074943359385415, -221.1585305289511041 ) ) ;
#8844 = CARTESIAN_POINT ( 'NONE',  ( -3.926352947695993745, 17.69140300707508473, -220.1607884481205986 ) ) ;
#8845 = CARTESIAN_POINT ( 'NONE',  ( 22.56777165119825668, 0.000000000000000000, 95.00000000000000000 ) ) ;
#8846 = CARTESIAN_POINT ( 'NONE',  ( 23.44063276014420794, 13.61134749381700182, -229.1061940987080732 ) ) ;
#8847 = CARTESIAN_POINT ( 'NONE',  ( -7.189383125363055349, 14.28512618638020548, -231.7475838278701303 ) ) ;
#8848 = CARTESIAN_POINT ( 'NONE',  ( -6.208492967940078877, 16.71913201805454463, -230.4912298573936766 ) ) ;
#8849 = CARTESIAN_POINT ( 'NONE',  ( 2.703362520412529779, 29.60004130108520215, -225.6165589735000481 ) ) ;
#8850 = CARTESIAN_POINT ( 'NONE',  ( -19.11923763334766946, 1.257783214997954202, -219.7591028439344711 ) ) ;
#8851 = CARTESIAN_POINT ( 'NONE',  ( 18.15173157547545557, 23.32481284044927961, -217.8532150843729482 ) ) ;
#8852 = CARTESIAN_POINT ( 'NONE',  ( 6.260833139380572732, -16.02228513277848876, -219.5457089733663736 ) ) ;
#8854 = DIRECTION ( 'NONE',  ( 1.401298464324817071E-45, 6.938893903907257960E-16, 1.000000000000000000 ) ) ;
#8853 = CIRCLE ( 'NONE', #21400, 21.00000000000008171 ) ;
#8855 = ORIENTED_EDGE ( 'NONE', *, *, #11743, .T. ) ;
#8856 = EDGE_CURVE ( 'NONE', #14290, #5879, #19973, .T. ) ;
#8857 = AXIS2_PLACEMENT_3D ( 'NONE', #3728, #21163, #19476 ) ;
#8858 = CARTESIAN_POINT ( 'NONE',  ( -10.45786516112131892, 23.61456281964591852, -233.2869923610001592 ) ) ;
#8859 = CARTESIAN_POINT ( 'NONE',  ( 23.75342044390781027, -1.773323855525749781, -231.1605140052801630 ) ) ;
#8860 = CARTESIAN_POINT ( 'NONE',  ( -1.232595164407830946E-29, 17.50000000000007105, -24.99999999999999645 ) ) ;
#8861 = CARTESIAN_POINT ( 'NONE',  ( 20.34032485158648029, 2.741617426884598530, -217.9827731991294968 ) ) ;
#8862 = CARTESIAN_POINT ( 'NONE',  ( -29.95012366401462955, 4.746560250930182967, -224.6954343660969471 ) ) ;
#8863 = CARTESIAN_POINT ( 'NONE',  ( 5.953549895739506326, -12.70069413479034104, -221.3143591192976203 ) ) ;
#8864 = CARTESIAN_POINT ( 'NONE',  ( -7.429838964355703901, 14.87322129099639234, -232.2632863647814077 ) ) ;
#8865 = ORIENTED_EDGE ( 'NONE', *, *, #13977, .T. ) ;
#8866 = CARTESIAN_POINT ( 'NONE',  ( -25.29098058636142810, 5.014641116111857144, -217.4658967307323110 ) ) ;
#8867 = CARTESIAN_POINT ( 'NONE',  ( -7.872599071444734697, -12.17161831996831367, -225.5779045487515191 ) ) ;
#8868 = DIRECTION ( 'NONE',  ( 0.000000000000000000, 0.000000000000000000, 1.000000000000000000 ) ) ;
#8869 = ADVANCED_FACE ( 'NONE', ( #13128 ), #11327, .F. ) ;
#8870 = DIRECTION ( 'NONE',  ( 0.000000000000000000, 0.000000000000000000, -1.000000000000000000 ) ) ;
#8871 = CARTESIAN_POINT ( 'NONE',  ( -13.98136146596813845, 3.850743984385103680, -228.7620665878280590 ) ) ;
#8872 = CARTESIAN_POINT ( 'NONE',  ( 13.74877878529187747, -9.499568690286848138, -221.9332727739125346 ) ) ;
#8873 = VECTOR ( 'NONE', #9920, 1000.000000000000000 ) ;
#8874 = CARTESIAN_POINT ( 'NONE',  ( 2.000000000000000000, 0.000000000000000000, -70.00000000000000000 ) ) ;
#8875 = CARTESIAN_POINT ( 'NONE',  ( 17.42772712443221650, 11.35756022693713341, -231.2166398222404382 ) ) ;
#8876 = CARTESIAN_POINT ( 'NONE',  ( -5.861205904341304951, 14.21969934012253312, -219.3213214613830644 ) ) ;
#8877 = CARTESIAN_POINT ( 'NONE',  ( 0.000000000000000000, 0.000000000000000000, -75.00000000000000000 ) ) ;
#8878 = CARTESIAN_POINT ( 'NONE',  ( 13.55451907249704213, 16.71566520821242818, -219.1474322952048226 ) ) ;
#8879 = CARTESIAN_POINT ( 'NONE',  ( -0.3443283949127196042, -14.50397496964243516, -224.4114361181996458 ) ) ;
#8880 = CARTESIAN_POINT ( 'NONE',  ( 30.27398588404266633, 0.3550328743180605762, -224.9805995843073561 ) ) ;
#8881 = EDGE_LOOP ( 'NONE', ( #1535, #12055, #2110, #9182 ) ) ;
#8882 = CARTESIAN_POINT ( 'NONE',  ( 22.69522586737246783, 3.669837464059151344, -234.0947686933411944 ) ) ;
#8883 = CARTESIAN_POINT ( 'NONE',  ( -4.715783688792956063, 28.29821729825949816, -228.0423900005874600 ) ) ;
#8884 = CARTESIAN_POINT ( 'NONE',  ( -21.47149190714903710, 3.672831083387290363, -231.0833634068433469 ) ) ;
#8885 = CARTESIAN_POINT ( 'NONE',  ( -20.49711526797010208, 7.006997077916217620, -215.3369776077118445 ) ) ;
#8886 = CARTESIAN_POINT ( 'NONE',  ( -14.27150057966913721, -8.785576370668652046, -221.5154223125717579 ) ) ;
#8887 = CARTESIAN_POINT ( 'NONE',  ( 1.526556658859590243E-13, -20.99999999999999645, -69.99999999999998579 ) ) ;
#8888 = ORIENTED_EDGE ( 'NONE', *, *, #8464, .T. ) ;
#8889 = CARTESIAN_POINT ( 'NONE',  ( 16.49791052269847569, 3.745513941566326999, -220.1874559167976884 ) ) ;
#8890 = CARTESIAN_POINT ( 'NONE',  ( 7.465087220526423373, -26.16405931560015219, -221.3372167714960312 ) ) ;
#8891 = CARTESIAN_POINT ( 'NONE',  ( 25.80927844399814930, 11.21489550116160316, -221.3538377621514996 ) ) ;
#8892 = CARTESIAN_POINT ( 'NONE',  ( -9.171998067665157350, 9.395241133357435714, -226.3428046914542051 ) ) ;
#8893 = CARTESIAN_POINT ( 'NONE',  ( 13.34963947135311102, 7.416462695144936390, -217.9359469527792044 ) ) ;
#8894 = CARTESIAN_POINT ( 'NONE',  ( 5.169766346882679997, 29.28517558595074988, -221.5178724947562614 ) ) ;
#8895 = CARTESIAN_POINT ( 'NONE',  ( -10.76827681573429984, 0.09137847850202132638, 92.00000000000000000 ) ) ;
#8896 = CARTESIAN_POINT ( 'NONE',  ( -1.542335193334551491, -19.71915426430242135, -216.1352730594569209 ) ) ;
#8897 = CARTESIAN_POINT ( 'NONE',  ( 24.80560757033128993, -15.22139526172250079, -221.3338856610240271 ) ) ;
#8898 = DIRECTION ( 'NONE',  ( -1.000000000000000000, 0.000000000000000000, 0.000000000000000000 ) ) ;
#8899 = DIRECTION ( 'NONE',  ( -1.000000000000000000, 0.000000000000000000, 0.000000000000000000 ) ) ;
#8900 = CARTESIAN_POINT ( 'NONE',  ( -8.716816145717144693, 12.22834664005217675, -231.7124508691059646 ) ) ;
#8901 = CARTESIAN_POINT ( 'NONE',  ( -22.93937586921525806, -8.311597057603599126, -230.3633560851501159 ) ) ;
#8902 = CARTESIAN_POINT ( 'NONE',  ( 26.75666476377482539, 8.100664119735744961, -232.1611550320539834 ) ) ;
#8903 = CARTESIAN_POINT ( 'NONE',  ( 5.955271202636533090, 21.50135983300913267, -233.0184468368920534 ) ) ;
#8904 = CARTESIAN_POINT ( 'NONE',  ( -1.248802714212398968, 14.93471382136348602, -228.4293827518713158 ) ) ;
#8905 = ORIENTED_EDGE ( 'NONE', *, *, #1573, .F. ) ;
#8906 = CARTESIAN_POINT ( 'NONE',  ( 15.43596206743521826, -16.12492210025319750, -235.0559386399467314 ) ) ;
#8907 = ORIENTED_EDGE ( 'NONE', *, *, #4003, .F. ) ;
#8908 = CARTESIAN_POINT ( 'NONE',  ( 24.42567939027770407, 10.22651298688739097, -219.4562066833365748 ) ) ;
#8909 = CARTESIAN_POINT ( 'NONE',  ( -12.99458409358603284, 11.56864380452031504, -232.0274663316965018 ) ) ;
#8910 = CARTESIAN_POINT ( 'NONE',  ( -13.01696012539752445, 9.878799299062107409, -218.8446158128127195 ) ) ;
#8911 = CARTESIAN_POINT ( 'NONE',  ( -30.29980174031923923, -2.072322947205907706, -221.9291348703773679 ) ) ;
#8912 = CARTESIAN_POINT ( 'NONE',  ( -9.151299407007059017, 9.196974979111923076, -223.9483834032048719 ) ) ;
#8913 = DIRECTION ( 'NONE',  ( 1.000000000000000000, 0.000000000000000000, 0.000000000000000000 ) ) ;
#8914 = DIRECTION ( 'NONE',  ( -1.000000000000000000, 0.000000000000000000, 0.000000000000000000 ) ) ;
#8915 = CARTESIAN_POINT ( 'NONE',  ( 13.10956039622986324, 4.581323766968698585, -221.0328522389722252 ) ) ;
#8916 = CARTESIAN_POINT ( 'NONE',  ( -9.852301241816233457, 15.10013604187968461, -230.8124578431014697 ) ) ;
#8917 = CARTESIAN_POINT ( 'NONE',  ( 8.681721411120292942, 8.442847255497570202, -228.0516816418615065 ) ) ;
#8918 = ADVANCED_FACE ( 'NONE', ( #4332 ), #1304, .T. ) ;
#8919 = CARTESIAN_POINT ( 'NONE',  ( -16.20072894238734307, 0.5024448614660336210, -230.4554067149722130 ) ) ;
#8920 = CARTESIAN_POINT ( 'NONE',  ( -12.58473846644578664, -2.158129970029659006, -220.6199603830026206 ) ) ;
#8921 = CARTESIAN_POINT ( 'NONE',  ( -13.83093441725390704, -7.146379636134302160, -230.0501880019394605 ) ) ;
#8922 = CARTESIAN_POINT ( 'NONE',  ( -9.350291727197115321, 27.53754332352430367, -230.1504993026967441 ) ) ;
#8923 = CARTESIAN_POINT ( 'NONE',  ( -3.734153817218577309, -19.72686645808614614, -233.9207428641194610 ) ) ;
#8924 = CARTESIAN_POINT ( 'NONE',  ( 5.017623471397871349, 29.83561274492976878, -222.9769172135417250 ) ) ;
#8925 = CARTESIAN_POINT ( 'NONE',  ( 4.248462565232024701, -14.07263755978623188, -232.0081791469470716 ) ) ;
#8926 = CARTESIAN_POINT ( 'NONE',  ( 0.000000000000000000, 0.000000000000000000, 77.51594804401857175 ) ) ;
#8927 = CARTESIAN_POINT ( 'NONE',  ( -29.22672729369577738, 6.588740615114764054, -224.9915299386302934 ) ) ;
#8928 = CARTESIAN_POINT ( 'NONE',  ( 0.9458336400950161371, 17.49535648476021876, -228.8359568483051589 ) ) ;
#8929 = CARTESIAN_POINT ( 'NONE',  ( 13.71882454279727526, 6.278400000045776252, -230.2269611870541723 ) ) ;
#8930 = CARTESIAN_POINT ( 'NONE',  ( 21.53262694368047647, 11.06794636811408594, -231.8394491640143826 ) ) ;
#8931 = CARTESIAN_POINT ( 'NONE',  ( 22.16968511661519869, 1.542591969257184337, -234.6098499860488573 ) ) ;
#8932 = CARTESIAN_POINT ( 'NONE',  ( -9.869267615102224056, -25.54258770546914903, -218.7733540664615930 ) ) ;
#8933 = CARTESIAN_POINT ( 'NONE',  ( 6.812728368504421539, 14.35307019806973194, -216.7766581591129977 ) ) ;
#8934 = DIRECTION ( 'NONE',  ( -1.000000000000000000, 0.000000000000000000, 0.000000000000000000 ) ) ;
#8935 = CARTESIAN_POINT ( 'NONE',  ( 2.018545692720245643, -30.97649562252411215, -224.4812544443210811 ) ) ;
#8936 = CARTESIAN_POINT ( 'NONE',  ( -9.810154340578240095, 25.84808829058669488, -220.5759521898573610 ) ) ;
#8937 = CARTESIAN_POINT ( 'NONE',  ( 6.040050017043670394, 13.67534390435379699, -220.4759402345340504 ) ) ;
#8938 = CARTESIAN_POINT ( 'NONE',  ( -27.09167109716269550, -0.2825935922571593539, -219.8389404328913486 ) ) ;
#8939 = CARTESIAN_POINT ( 'NONE',  ( -15.95412330064426065, 13.09400588185824077, -218.6613039563597169 ) ) ;
#8940 = EDGE_CURVE ( 'NONE', #2515, #3746, #19853, .T. ) ;
#8941 = AXIS2_PLACEMENT_3D ( 'NONE', #11336, #8078, #17986 ) ;
#8942 = CARTESIAN_POINT ( 'NONE',  ( -13.24620988741752825, 28.78239319002125285, -225.3527830703614256 ) ) ;
#8943 = CARTESIAN_POINT ( 'NONE',  ( 22.42095341476093040, 9.457779162868732215, -232.6339572190428555 ) ) ;
#8944 = EDGE_LOOP ( 'NONE', ( #12143, #414, #16206, #20787, #17415 ) ) ;
#8945 = CARTESIAN_POINT ( 'NONE',  ( 15.57652300565637482, -15.79620443381692496, -231.0117242343698081 ) ) ;
#8946 = CARTESIAN_POINT ( 'NONE',  ( 17.47229821656412341, -21.26691171910925249, -219.4940788861217413 ) ) ;
#8947 = CARTESIAN_POINT ( 'NONE',  ( -2.993956627714193353, 22.04778837082692178, -231.1741803919495339 ) ) ;
#8948 = EDGE_LOOP ( 'NONE', ( #12915, #10235, #13161, #15879 ) ) ;
#8949 = DIRECTION ( 'NONE',  ( -1.000000000000000000, 0.000000000000000000, 0.000000000000000000 ) ) ;
#8950 = CARTESIAN_POINT ( 'NONE',  ( 10.83706092800007781, 10.12544885278926543, -227.1716144446442343 ) ) ;
#8951 = CARTESIAN_POINT ( 'NONE',  ( -27.06886705769815649, 1.548837563602061262, -218.3554811309518868 ) ) ;
#8952 = CARTESIAN_POINT ( 'NONE',  ( -24.92024473536680773, -13.74570206812420103, -220.1598944320903115 ) ) ;
#8953 = CARTESIAN_POINT ( 'NONE',  ( -2.576162127940193169, -15.57202066281789321, -231.6911579627040396 ) ) ;
#8954 = CARTESIAN_POINT ( 'NONE',  ( 0.1979841192334154676, 16.22068729745496540, -223.9539336445596973 ) ) ;
#8955 = DIRECTION ( 'NONE',  ( -0.000000000000000000, -0.000000000000000000, -1.000000000000000000 ) ) ;
#8956 = CARTESIAN_POINT ( 'NONE',  ( 25.01541028746040141, 13.78427203520734423, -225.9266837950359843 ) ) ;
#8957 = CARTESIAN_POINT ( 'NONE',  ( -3.060450601941519189, 13.29454208326677289, -222.0135664617158682 ) ) ;
#8958 = CARTESIAN_POINT ( 'NONE',  ( -6.573387563318148885, 17.69612765735440973, -231.1211991061559274 ) ) ;
#8959 = CARTESIAN_POINT ( 'NONE',  ( 2.785859284650920031, 14.19821255961969619, -226.9946081512528906 ) ) ;
#8960 = CARTESIAN_POINT ( 'NONE',  ( -16.27736488614644372, 5.941157768540612949, -228.4237983497913547 ) ) ;
#8961 = CARTESIAN_POINT ( 'NONE',  ( 29.64577750251057608, 2.839131411071813549, -220.9704389295326905 ) ) ;
#8962 = CARTESIAN_POINT ( 'NONE',  ( 5.511302051500400090, -18.01881380728196902, -231.5522404100356084 ) ) ;
#8963 = CARTESIAN_POINT ( 'NONE',  ( 13.63685685255378743, 0.3474052042451960531, -228.2001920571242124 ) ) ;
#8964 = DIRECTION ( 'NONE',  ( 0.000000000000000000, 0.000000000000000000, -1.000000000000000000 ) ) ;
#8965 = CARTESIAN_POINT ( 'NONE',  ( 7.168644370073567806, 19.32044210858112265, -233.1278450877711634 ) ) ;
#8966 = CARTESIAN_POINT ( 'NONE',  ( 17.78543650172321833, -3.538499054913423869, -220.4382406111031401 ) ) ;
#8967 = CARTESIAN_POINT ( 'NONE',  ( 26.00000000000000000, 1.360023205165816762E-13, 0.000000000000000000 ) ) ;
#8968 = CARTESIAN_POINT ( 'NONE',  ( 18.76922974182421555, 13.12635134380198210, -217.8010375391909008 ) ) ;
#8969 = CARTESIAN_POINT ( 'NONE',  ( 8.257114973007913861, -25.39836461225790742, -232.6217252414676295 ) ) ;
#8970 = FILL_AREA_STYLE_COLOUR ( '', #16000 ) ;
#8971 = CARTESIAN_POINT ( 'NONE',  ( -15.66530208164916260, 23.23467148471576849, -218.1250122661128046 ) ) ;
#8972 = ADVANCED_FACE ( 'NONE', ( #6474 ), #3093, .F. ) ;
#8973 = CARTESIAN_POINT ( 'NONE',  ( -19.18087294808806931, 21.32275554655070593, -230.8558978902391061 ) ) ;
#8974 = ORIENTED_EDGE ( 'NONE', *, *, #5496, .T. ) ;
#8975 = CARTESIAN_POINT ( 'NONE',  ( -13.69675006931110417, 3.702342960760605539, -228.0723273272095355 ) ) ;
#8976 = CARTESIAN_POINT ( 'NONE',  ( -11.55581979318669639, -19.97716813486601239, -217.5317483122086912 ) ) ;
#8977 = CARTESIAN_POINT ( 'NONE',  ( -25.00000000000013500, 6.609496070381316956E-17, -10.00000000000000000 ) ) ;
#8978 = CARTESIAN_POINT ( 'NONE',  ( -23.00000000000000355, 0.3295946125619286238, 10.00000000000000000 ) ) ;
#8979 = CARTESIAN_POINT ( 'NONE',  ( -13.69675006931110417, 3.702342960760605539, -228.0723273272095355 ) ) ;
#8980 = CARTESIAN_POINT ( 'NONE',  ( 3.247425482496454130, -26.49846316390620160, -232.4805733197358677 ) ) ;
#8982 = EDGE_CURVE ( 'NONE', #12667, #4483, #12329, .T. ) ;
#8981 = LINE ( 'NONE', #14488, #2721 ) ;
#8983 = FACE_OUTER_BOUND ( 'NONE', #22238, .T. ) ;
#8984 = CARTESIAN_POINT ( 'NONE',  ( 22.37742875470728876, 11.29804624588327577, -218.9256858961603882 ) ) ;
#8985 = CARTESIAN_POINT ( 'NONE',  ( -21.50655177804914686, 20.61731362457859973, -218.7935603611527426 ) ) ;
#8986 = DIRECTION ( 'NONE',  ( 0.000000000000000000, 0.000000000000000000, 1.000000000000000000 ) ) ;
#8987 = CARTESIAN_POINT ( 'NONE',  ( 25.01541028746040141, 13.78427203520734423, -225.9266837950359843 ) ) ;
#8988 = CARTESIAN_POINT ( 'NONE',  ( 2.219167932009094901, -23.00164214691015729, -217.1940376169840476 ) ) ;
#8989 = ORIENTED_EDGE ( 'NONE', *, *, #22191, .T. ) ;
#8990 = CARTESIAN_POINT ( 'NONE',  ( -4.067324790461362305, 15.10342260507846746, -228.2464404076259257 ) ) ;
#8991 = CARTESIAN_POINT ( 'NONE',  ( -13.58070052954164275, 11.19572749768420650, -220.2511552028196604 ) ) ;
#8992 = CARTESIAN_POINT ( 'NONE',  ( 15.58465056415575312, 2.812367138262562349, -229.5090343034091234 ) ) ;
#8993 = CARTESIAN_POINT ( 'NONE',  ( -15.14636561941736481, -8.091785236158230532, -228.8632199501622608 ) ) ;
#8994 = FACE_OUTER_BOUND ( 'NONE', #13948, .T. ) ;
#8995 = ORIENTED_EDGE ( 'NONE', *, *, #20384, .F. ) ;
#8996 = CARTESIAN_POINT ( 'NONE',  ( 23.83082175545800752, 15.77842900014857896, -219.5351905769044834 ) ) ;
#8997 = CARTESIAN_POINT ( 'NONE',  ( 6.629309777743229937, -15.42610274396934855, -227.9597969125812256 ) ) ;
#8998 = CARTESIAN_POINT ( 'NONE',  ( 22.66390650824515873, 11.48342577402021725, -231.3155567808436217 ) ) ;
#8999 = CARTESIAN_POINT ( 'NONE',  ( -22.99617382825321599, 17.18101613848176967, -230.9512687019100099 ) ) ;
#9000 = CARTESIAN_POINT ( 'NONE',  ( 17.96045420455031305, -0.3746358454349600908, -217.9627609769914613 ) ) ;
#9001 = CARTESIAN_POINT ( 'NONE',  ( 0.9908753270255351575, 13.79205759140780430, -228.0165926715089881 ) ) ;
#9002 = CARTESIAN_POINT ( 'NONE',  ( 13.39702356564321306, 1.314794804900859537, -222.2999924150924187 ) ) ;
#9003 = CARTESIAN_POINT ( 'NONE',  ( -7.531388159411753769, -21.98719092781708540, -216.0713624712111312 ) ) ;
#9004 = CARTESIAN_POINT ( 'NONE',  ( 12.31511859722645852, -8.491226738247512174, -220.9006323875693738 ) ) ;
#9005 = PLANE ( 'NONE',  #19575 ) ;
#9006 = DIRECTION ( 'NONE',  ( 0.000000000000000000, 0.000000000000000000, -1.000000000000000000 ) ) ;
#9007 = CARTESIAN_POINT ( 'NONE',  ( -7.686214453470440411, 10.71593237010305444, -228.8058998235944159 ) ) ;
#9008 = CARTESIAN_POINT ( 'NONE',  ( -18.92071285517992507, -7.235402657652117320, -230.6453433565968680 ) ) ;
#9009 = CARTESIAN_POINT ( 'NONE',  ( -12.62195384480319582, 9.244619650382723819, -228.6283004876635516 ) ) ;
#9010 = CARTESIAN_POINT ( 'NONE',  ( 8.860681144154234801, 27.11956268701432293, -229.8503778060109823 ) ) ;
#9011 = CARTESIAN_POINT ( 'NONE',  ( -0.7292515499105728383, 28.18841485102515776, -220.8637599502617093 ) ) ;
#9012 = EDGE_LOOP ( 'NONE', ( #12937, #11784, #5188, #3525, #14348, #14255 ) ) ;
#9013 = CARTESIAN_POINT ( 'NONE',  ( 26.46513128492211564, -16.79977778982552650, -229.3906297761492681 ) ) ;
#9014 = VERTEX_POINT ( 'NONE', #2978 ) ;
#9015 = CARTESIAN_POINT ( 'NONE',  ( 13.03557269046774714, 7.519834803053426775, -226.9490612297269081 ) ) ;
#9016 = CARTESIAN_POINT ( 'NONE',  ( -11.40916210110096962, 20.01996232974788725, -234.3205435716851923 ) ) ;
#9017 = CARTESIAN_POINT ( 'NONE',  ( -16.09559989144903369, 12.31939076846282966, -216.7948290530243298 ) ) ;
#9018 = CARTESIAN_POINT ( 'NONE',  ( -15.92941692657317354, -7.780888323563449838, -232.0381278758927976 ) ) ;
#9019 = ADVANCED_FACE ( 'NONE', ( #9640 ), #5402, .F. ) ;
#9020 = CARTESIAN_POINT ( 'NONE',  ( -17.79285498209129202, 9.187865686019035749, -216.3798185811636756 ) ) ;
#9021 = CLOSED_SHELL ( 'NONE', ( #15347, #18775, #11417, #1620, #9019, #12924, #6565, #19148, #11460, #16952 ) ) ;
#9022 = DIRECTION ( 'NONE',  ( -0.000000000000000000, 0.000000000000000000, -1.000000000000000000 ) ) ;
#9023 = ADVANCED_FACE ( 'NONE', ( #3182 ), #3330, .F. ) ;
#9024 = CARTESIAN_POINT ( 'NONE',  ( 12.25122766587143630, 4.035812653434439845, -225.7709573147497224 ) ) ;
#9025 = CARTESIAN_POINT ( 'NONE',  ( -9.969679877803788060, 12.84542071557917176, -220.4758784541224657 ) ) ;
#9026 = CARTESIAN_POINT ( 'NONE',  ( 19.48863273024974418, 12.80680990455712909, -215.0408095016468053 ) ) ;
#9027 = CARTESIAN_POINT ( 'NONE',  ( -13.98136146596813845, 3.850743984385103680, -228.7620665878280590 ) ) ;
#9028 = CARTESIAN_POINT ( 'NONE',  ( -20.48546531633906298, -12.23885716989380157, -214.8851912114337210 ) ) ;
#9029 = CARTESIAN_POINT ( 'NONE',  ( -30.29980174031923923, -2.072322947205907706, -221.9291348703773679 ) ) ;
#9030 = CARTESIAN_POINT ( 'NONE',  ( 2.482746429915354547, 16.41797261123590346, -229.5599230346982154 ) ) ;
#9031 = CARTESIAN_POINT ( 'NONE',  ( -6.870552667427666904, -18.85419487977974029, -216.2130481585807047 ) ) ;
#9032 = CARTESIAN_POINT ( 'NONE',  ( 12.04687593227112430, 27.54339840196571743, -224.6466266724203820 ) ) ;
#9033 = CARTESIAN_POINT ( 'NONE',  ( 11.86117213253061387, -14.68998886196529874, -215.0859965227146802 ) ) ;
#9034 = PLANE ( 'NONE',  #12451 ) ;
#9035 = CARTESIAN_POINT ( 'NONE',  ( -18.14952719657095415, 1.368063294522122275, -218.0005379682515922 ) ) ;
#9036 = DIRECTION ( 'NONE',  ( -1.000000000000000000, 0.000000000000000000, 0.000000000000000000 ) ) ;
#9037 = CARTESIAN_POINT ( 'NONE',  ( -2.532302712337851425, 16.54370602006230939, -228.1940632970506613 ) ) ;
#9038 = CARTESIAN_POINT ( 'NONE',  ( 16.48801037644500056, 3.165716804515234628, -216.8169430726136113 ) ) ;
#9039 = CARTESIAN_POINT ( 'NONE',  ( 26.24002132888527328, 11.62331517472360964, -222.5300873157218859 ) ) ;
#9040 = CARTESIAN_POINT ( 'NONE',  ( 24.20411255886326529, 12.66254860825103634, -218.0144359054998802 ) ) ;
#9041 = CARTESIAN_POINT ( 'NONE',  ( -5.646690751453034451, -19.25001164140187981, -233.5706237494638913 ) ) ;
#9042 = CARTESIAN_POINT ( 'NONE',  ( 2.804048525646705148, 30.59371477727813726, -220.6614663749232363 ) ) ;
#9043 = DIRECTION ( 'NONE',  ( 1.000000000000000000, 0.000000000000000000, 0.000000000000000000 ) ) ;
#9044 = CARTESIAN_POINT ( 'NONE',  ( -4.398080837965281376, -27.92536303359771566, -232.3360949592949112 ) ) ;
#9045 = CARTESIAN_POINT ( 'NONE',  ( -4.691002462566371101, 21.98518063340150164, -232.2516024630330094 ) ) ;
#9046 = CARTESIAN_POINT ( 'NONE',  ( 15.26539804565921621, 9.309431686815628382, -232.9129599938668207 ) ) ;
#9047 = CARTESIAN_POINT ( 'NONE',  ( -12.69709334397052203, 10.59859500067950400, -221.6107941937004568 ) ) ;
#9048 = CARTESIAN_POINT ( 'NONE',  ( -4.378220565073127624, 31.53459173284372952, -222.0564199190954753 ) ) ;
#9049 = CARTESIAN_POINT ( 'NONE',  ( 26.53121369294028042, 10.74560293343441586, -229.2288136770759195 ) ) ;
#9050 = CARTESIAN_POINT ( 'NONE',  ( 18.44909377000590922, -20.66544815256419199, -223.5047567001167863 ) ) ;
#9051 = EDGE_LOOP ( 'NONE', ( #6991, #21546, #11916, #8507 ) ) ;
#9052 = CARTESIAN_POINT ( 'NONE',  ( 7.876378987416962296, -12.17572650474792617, -223.4643623724329018 ) ) ;
#9053 = CARTESIAN_POINT ( 'NONE',  ( -5.706122936196527107, 15.14201253431006045, -228.6865785740211550 ) ) ;
#9054 = PRODUCT_RELATED_PRODUCT_CATEGORY ( 'part', '', ( #16966 ) ) ;
#9055 = CARTESIAN_POINT ( 'NONE',  ( -24.63401512838757768, 0.000000000000000000, -77.51594804401857175 ) ) ;
#9056 = AXIS2_PLACEMENT_3D ( 'NONE', #18392, #19733, #14915 ) ;
#9057 = CARTESIAN_POINT ( 'NONE',  ( 17.97843143658897347, 22.12221935793617078, -220.9346589834416079 ) ) ;
#9058 = CARTESIAN_POINT ( 'NONE',  ( 28.33476664927451338, -0.7768526459456059907, -228.3750448408243869 ) ) ;
#9059 = CARTESIAN_POINT ( 'NONE',  ( -14.76273180397945772, -6.370707202906876532, -220.0066229284273334 ) ) ;
#9060 = CARTESIAN_POINT ( 'NONE',  ( 2.378655016347637652, -14.31292064579845302, -219.9942319014987220 ) ) ;
#9061 = CARTESIAN_POINT ( 'NONE',  ( -1.158668551263366986, 23.31492692626720853, -219.2372600964201865 ) ) ;
#9062 = DIRECTION ( 'NONE',  ( -1.000000000000000000, 0.000000000000000000, 0.000000000000000000 ) ) ;
#9063 = CARTESIAN_POINT ( 'NONE',  ( 27.30736127486511577, 7.960716467858479639, -228.6121938484450595 ) ) ;
#9064 = CARTESIAN_POINT ( 'NONE',  ( -18.47334320050258327, 24.79293862780133040, -226.9986786077537317 ) ) ;
#9065 = CARTESIAN_POINT ( 'NONE',  ( -11.11821474075380678, 16.53100589793018926, -232.3736596382188395 ) ) ;
#9066 = TOROIDAL_SURFACE ( 'NONE', #2919, 12.50000000000000355, 5.000000000000000000 ) ;
#9067 = CARTESIAN_POINT ( 'NONE',  ( 7.213476267053916757, 16.78447451494783138, -217.5857052077849687 ) ) ;
#9068 = CARTESIAN_POINT ( 'NONE',  ( -21.18474081038989354, 8.486062504918864491, -230.7949373529753530 ) ) ;
#9069 = CARTESIAN_POINT ( 'NONE',  ( 21.06229272850552547, 3.434461253538921621, -234.1452885155528918 ) ) ;
#9070 = CARTESIAN_POINT ( 'NONE',  ( 9.020349274477036161, -13.22217574948208529, -220.4173403795374213 ) ) ;
#9071 = DIRECTION ( 'NONE',  ( -2.162300680179923768E-16, -1.000000000000000000, 0.000000000000000000 ) ) ;
#9072 = ORIENTED_EDGE ( 'NONE', *, *, #14496, .T. ) ;
#9073 = CARTESIAN_POINT ( 'NONE',  ( 4.883314309504700468, 19.06839645569368358, -217.0171359871271193 ) ) ;
#9074 = CARTESIAN_POINT ( 'NONE',  ( 25.63739587761438088, -9.098054415140415685, -222.2988516439644968 ) ) ;
#9075 = LINE ( 'NONE', #10430, #20545 ) ;
#9076 = CIRCLE ( 'NONE', #19480, 3.000000000000002665 ) ;
#9077 = CARTESIAN_POINT ( 'NONE',  ( 21.31262902390056624, 0.4111834581965390645, -232.0572713672585792 ) ) ;
#9078 = CARTESIAN_POINT ( 'NONE',  ( 0.7326557587344989519, -29.96088689026728602, -229.4725774697800205 ) ) ;
#9079 = CARTESIAN_POINT ( 'NONE',  ( 0.000000000000000000, 0.000000000000000000, 0.000000000000000000 ) ) ;
#9080 = CARTESIAN_POINT ( 'NONE',  ( -20.18153419852512442, 14.25141268122526483, -233.5059133483111964 ) ) ;
#9081 = CARTESIAN_POINT ( 'NONE',  ( -16.28135616697389310, 20.98764039357472200, -216.9434553755565958 ) ) ;
#9082 = CARTESIAN_POINT ( 'NONE',  ( -14.87984907657228639, 0.2138881189739126887, -228.7773920408832282 ) ) ;
#9083 = CARTESIAN_POINT ( 'NONE',  ( -12.35609710479046441, -10.83622032031252758, -230.4552079900997228 ) ) ;
#9084 = CARTESIAN_POINT ( 'NONE',  ( 0.000000000000000000, 0.000000000000000000, -70.00000000000000000 ) ) ;
#9085 = CARTESIAN_POINT ( 'NONE',  ( -27.90314475660494153, 12.48829126175061077, -223.3300566725355338 ) ) ;
#9086 = CARTESIAN_POINT ( 'NONE',  ( 9.500235314199413139, -15.98409598254677455, -218.3811512014305265 ) ) ;
#9087 = CIRCLE ( 'NONE', #15213, 3.000000000000002665 ) ;
#9088 = DIRECTION ( 'NONE',  ( -1.000000000000000000, 0.000000000000000000, 0.000000000000000000 ) ) ;
#9089 = ADVANCED_FACE ( 'NONE', ( #1829 ), #6192, .T. ) ;
#9090 = AXIS2_PLACEMENT_3D ( 'NONE', #5722, #8790, #9117 ) ;
#9091 = CARTESIAN_POINT ( 'NONE',  ( 16.23850682336481199, 8.051046992137072422, -219.2473483181185827 ) ) ;
#9092 = CARTESIAN_POINT ( 'NONE',  ( -7.626320092023432196, 21.25423560278784407, -233.8867968595558295 ) ) ;
#9093 = DIRECTION ( 'NONE',  ( -0.000000000000000000, -0.000000000000000000, -1.000000000000000000 ) ) ;
#9094 = CARTESIAN_POINT ( 'NONE',  ( 12.60818910183731489, 13.02403301690871729, -229.3305689548085695 ) ) ;
#9095 = CARTESIAN_POINT ( 'NONE',  ( -6.479026444546563290, -23.11309618162032820, -231.4158670874050756 ) ) ;
#9096 = ORIENTED_EDGE ( 'NONE', *, *, #7973, .F. ) ;
#9097 = CARTESIAN_POINT ( 'NONE',  ( -5.365396334125453137, 16.47374957271378904, -219.4721119688156534 ) ) ;
#9098 = CARTESIAN_POINT ( 'NONE',  ( -17.65560862077320081, 21.92186454631220371, -221.3776075196718693 ) ) ;
#9099 = CARTESIAN_POINT ( 'NONE',  ( -31.12406087576577463, 7.316399946619934092, -225.0171288978685027 ) ) ;
#9100 = ORIENTED_EDGE ( 'NONE', *, *, #357, .F. ) ;
#9101 = CARTESIAN_POINT ( 'NONE',  ( -17.99186107021003167, -20.03292934477192944, -228.1636640080403424 ) ) ;
#9102 = CARTESIAN_POINT ( 'NONE',  ( 22.56777165119825668, 0.000000000000000000, 90.00000000000000000 ) ) ;
#9103 = VERTEX_POINT ( 'NONE', #18726 ) ;
#9104 = CARTESIAN_POINT ( 'NONE',  ( -28.59157645096996347, 5.137867505054540374, -220.4667042235044505 ) ) ;
#9105 = CARTESIAN_POINT ( 'NONE',  ( 7.724698117049915602, -20.76727510557136469, -231.0612438369181518 ) ) ;
#9106 = CARTESIAN_POINT ( 'NONE',  ( 17.00168025137501004, 6.212099629982537508, -219.0548246536471595 ) ) ;
#9107 = CARTESIAN_POINT ( 'NONE',  ( 4.883314309504700468, 19.06839645569368358, -217.0171359871271193 ) ) ;
#9108 = CIRCLE ( 'NONE', #21657, 16.02266676603872142 ) ;
#9109 = EDGE_CURVE ( 'NONE', #7880, #17843, #2607, .T. ) ;
#9110 = VECTOR ( 'NONE', #18442, 1000.000000000000000 ) ;
#9111 = CARTESIAN_POINT ( 'NONE',  ( -21.16281446184100545, 3.810576631694648775, -218.4455094643457187 ) ) ;
#9112 = CARTESIAN_POINT ( 'NONE',  ( 8.329997790135040603, 12.51216704542961899, -228.7022893680961602 ) ) ;
#9113 = CARTESIAN_POINT ( 'NONE',  ( 25.50000000000000000, -4.400000000000000355, -3.299999999999998490 ) ) ;
#9114 = CARTESIAN_POINT ( 'NONE',  ( -6.052919920376759855, -15.38051382379660836, -218.0337201863237624 ) ) ;
#9115 = CARTESIAN_POINT ( 'NONE',  ( 18.55298002304457228, -12.22359628793950570, -216.9137843736221782 ) ) ;
#9116 = CARTESIAN_POINT ( 'NONE',  ( 0.000000000000000000, 0.000000000000000000, 78.50000000000000000 ) ) ;
#9117 = DIRECTION ( 'NONE',  ( 1.000000000000000000, 0.000000000000000000, 0.000000000000000000 ) ) ;
#9118 = CARTESIAN_POINT ( 'NONE',  ( -11.10150084103673684, 3.549415896002023896, -226.0408865487038952 ) ) ;
#9119 = CARTESIAN_POINT ( 'NONE',  ( -22.88587990158785601, -12.52061884883742238, -220.5813279352508687 ) ) ;
#9120 = AXIS2_PLACEMENT_3D ( 'NONE', #5718, #19114, #2343 ) ;
#9121 = AXIS2_PLACEMENT_3D ( 'NONE', #20436, #6840, #6731 ) ;
#9122 = CARTESIAN_POINT ( 'NONE',  ( -18.94992041651601156, 14.87246523864368974, -232.0280096192260828 ) ) ;
#9123 = CARTESIAN_POINT ( 'NONE',  ( 13.48097272627202159, 8.509510470709432894, -231.5257201610278059 ) ) ;
#9124 = CARTESIAN_POINT ( 'NONE',  ( -1.582540545905128049, 14.52388882916313584, -222.9138157219475147 ) ) ;
#9125 = ORIENTED_EDGE ( 'NONE', *, *, #6671, .F. ) ;
#9126 = CARTESIAN_POINT ( 'NONE',  ( 15.68748001070188458, -20.89997441943167900, -216.2583427777263125 ) ) ;
#9127 = ORIENTED_EDGE ( 'NONE', *, *, #2914, .T. ) ;
#9128 = CARTESIAN_POINT ( 'NONE',  ( 14.32085100525799248, 9.220655089380342062, -219.9006227404039464 ) ) ;
#9129 = CARTESIAN_POINT ( 'NONE',  ( -5.340143745732740754, 22.10628181454592678, -235.0476201740528097 ) ) ;
#9130 = CARTESIAN_POINT ( 'NONE',  ( -8.123851230256436295, 20.56863949923577550, -215.0796075421103239 ) ) ;
#9131 = CARTESIAN_POINT ( 'NONE',  ( -12.88620494227545343, -3.269292211592822461, -225.1464181993036391 ) ) ;
#9132 = CARTESIAN_POINT ( 'NONE',  ( -11.67631226053870996, 6.737291529340801333, -227.3110382950315227 ) ) ;
#9133 = FACE_OUTER_BOUND ( 'NONE', #18914, .T. ) ;
#9134 = EDGE_CURVE ( 'NONE', #9986, #14013, #18790, .T. ) ;
#9135 = CARTESIAN_POINT ( 'NONE',  ( 0.000000000000000000, 0.000000000000000000, -55.00000000000000000 ) ) ;
#9136 = CONICAL_SURFACE ( 'NONE', #19889, 25.00000000000001066, 0.2617993877991500740 ) ;
#9137 = CARTESIAN_POINT ( 'NONE',  ( -12.69709334397052203, 10.59859500067950400, -221.6107941937004568 ) ) ;
#9138 = CARTESIAN_POINT ( 'NONE',  ( 18.50073117969547098, -1.889592114545683987, -232.6396648696776026 ) ) ;
#9139 = CARTESIAN_POINT ( 'NONE',  ( -15.15110768032078070, 3.517015312212880218, -219.5479300368539270 ) ) ;
#9140 = VECTOR ( 'NONE', #20548, 1000.000000000000000 ) ;
#9141 = CARTESIAN_POINT ( 'NONE',  ( 11.57669841200422134, 10.63052136557218574, -228.9489978335593889 ) ) ;
#9142 = CARTESIAN_POINT ( 'NONE',  ( -22.25980993584449408, -3.522148912989541802, -233.7954546715351398 ) ) ;
#9143 = EDGE_CURVE ( 'NONE', #15940, #3760, #9087, .T. ) ;
#9144 = CARTESIAN_POINT ( 'NONE',  ( 1.313727069624702981, 17.80710275190598324, -219.4197901500037062 ) ) ;
#9145 = CARTESIAN_POINT ( 'NONE',  ( -6.512931564893298386, -17.32529878264574563, -216.7284160531958719 ) ) ;
#9146 = CARTESIAN_POINT ( 'NONE',  ( 17.19674704922021391, 23.07334190050143974, -228.8256488842130238 ) ) ;
#9147 = CARTESIAN_POINT ( 'NONE',  ( 7.117641012966415381, -28.94820313438933113, -231.4073019955615393 ) ) ;
#9148 = LINE ( 'NONE', #17478, #929 ) ;
#9149 = CARTESIAN_POINT ( 'NONE',  ( -14.94667331530454213, 6.325011500478772142, -230.0242139990887154 ) ) ;
#9150 = CARTESIAN_POINT ( 'NONE',  ( 15.07245478799217686, -4.018468087397350175, -231.0118529037252699 ) ) ;
#9151 = CARTESIAN_POINT ( 'NONE',  ( 7.804112641607792611, 19.76858558208418515, -218.6463059509973164 ) ) ;
#9152 = CARTESIAN_POINT ( 'NONE',  ( -16.81936022032888545, 5.700806722825413786, -218.5726178058217215 ) ) ;
#9153 = CARTESIAN_POINT ( 'NONE',  ( 20.58703255433590940, 0.4816031003617209372, -231.9427175861361263 ) ) ;
#9154 = CARTESIAN_POINT ( 'NONE',  ( -11.33724117040414647, -11.57131516804904159, -228.9094961685112537 ) ) ;
#9155 = ADVANCED_FACE ( 'NONE', ( #13781 ), #20619, .T. ) ;
#9156 = CARTESIAN_POINT ( 'NONE',  ( 14.75291830987536557, 13.43762972591284033, -235.1407057970265839 ) ) ;
#9157 = CIRCLE ( 'NONE', #21355, 25.00000000000010303 ) ;
#9158 = CARTESIAN_POINT ( 'NONE',  ( 0.000000000000000000, 0.000000000000000000, -77.51594804401857175 ) ) ;
#9159 = CARTESIAN_POINT ( 'NONE',  ( -3.456580335739853016, -11.82839499582713749, -226.8096787805597501 ) ) ;
#9160 = CARTESIAN_POINT ( 'NONE',  ( -8.030397104878142400, 15.90963402996711373, -230.6518438502475590 ) ) ;
#9161 = CARTESIAN_POINT ( 'NONE',  ( 8.821742718405863215, 10.82866050966069160, -221.4785132813277642 ) ) ;
#9162 = CARTESIAN_POINT ( 'NONE',  ( -14.20363567091065349, 7.857660128015216294, -223.4151327167956822 ) ) ;
#9163 = CARTESIAN_POINT ( 'NONE',  ( -10.30034651166687887, 25.05454868506992838, -216.5587736482213188 ) ) ;
#9164 = CARTESIAN_POINT ( 'NONE',  ( 14.21126657910812874, 6.833562750302326627, -220.2783117037562874 ) ) ;
#9165 = ORIENTED_EDGE ( 'NONE', *, *, #4443, .F. ) ;
#9166 = CARTESIAN_POINT ( 'NONE',  ( 10.74448773353722686, -20.82765299830942851, -219.2305132457354659 ) ) ;
#9167 = VERTEX_POINT ( 'NONE', #153 ) ;
#9168 = CARTESIAN_POINT ( 'NONE',  ( 9.009845654114897684, -15.13764346805314354, -231.2790349225496129 ) ) ;
#9169 = CARTESIAN_POINT ( 'NONE',  ( -5.764806379010653181, 14.19340719117484007, -223.8851086052821415 ) ) ;
#9170 = ORIENTED_EDGE ( 'NONE', *, *, #15073, .T. ) ;
#9171 = CARTESIAN_POINT ( 'NONE',  ( 25.50000000000000000, 4.399999999999999467, -3.300000000000000266 ) ) ;
#9172 = AXIS2_PLACEMENT_3D ( 'NONE', #1582, #1793, #18467 ) ;
#9173 = CARTESIAN_POINT ( 'NONE',  ( 27.40550551777678123, 5.967061366481472895, -228.7463788799179554 ) ) ;
#9174 = CARTESIAN_POINT ( 'NONE',  ( 23.12216041205843453, 0.2121350054995089496, -232.0572713672589202 ) ) ;
#9175 = CARTESIAN_POINT ( 'NONE',  ( -15.27057301462635408, -17.00912219741827514, -233.6288396447818627 ) ) ;
#9176 = CARTESIAN_POINT ( 'NONE',  ( -7.531388159411753769, -21.98719092781708540, -216.0713624712111312 ) ) ;
#9177 = CARTESIAN_POINT ( 'NONE',  ( 9.094331215210646135, 23.85463374792894342, -219.7669638091879847 ) ) ;
#9178 = CARTESIAN_POINT ( 'NONE',  ( -17.50000000000001066, 2.143131898507869431E-15, -55.00000000000000711 ) ) ;
#9179 = CARTESIAN_POINT ( 'NONE',  ( -29.98527381603928887, 6.316825171121390525, -230.1108345570740994 ) ) ;
#9180 = CARTESIAN_POINT ( 'NONE',  ( -9.749377714296398878, 10.28442384816749922, -229.3722863967025205 ) ) ;
#9181 = CARTESIAN_POINT ( 'NONE',  ( 3.528957931946373971, 27.43889307663531696, -223.4805233499528185 ) ) ;
#9182 = ORIENTED_EDGE ( 'NONE', *, *, #21371, .F. ) ;
#9183 = CARTESIAN_POINT ( 'NONE',  ( 5.833753951408669813, 12.47745132051510453, -226.2508980627489450 ) ) ;
#9184 = CARTESIAN_POINT ( 'NONE',  ( -24.48812334466693486, 4.469247780253509106, -230.3044243311433945 ) ) ;
#9185 = CARTESIAN_POINT ( 'NONE',  ( 12.08790845148079640, 6.355304031620478078, -220.0087475230167229 ) ) ;
#9186 = CARTESIAN_POINT ( 'NONE',  ( 10.46316887740464985, -17.92901728017801233, -232.6108895528913081 ) ) ;
#9187 = DIRECTION ( 'NONE',  ( -1.000000000000000000, 0.000000000000000000, -0.000000000000000000 ) ) ;
#9188 = ORIENTED_EDGE ( 'NONE', *, *, #3918, .F. ) ;
#9189 = CARTESIAN_POINT ( 'NONE',  ( 8.812073984913094904, 13.12649198322903210, -229.9172071780580495 ) ) ;
#9190 = CARTESIAN_POINT ( 'NONE',  ( -22.13988250630526267, 1.271659148212506141, -215.1660654604927458 ) ) ;
#9191 = CARTESIAN_POINT ( 'NONE',  ( 0.000000000000000000, 0.000000000000000000, 75.34729635533385306 ) ) ;
#9192 = CIRCLE ( 'NONE', #21025, 5.500000000000000000 ) ;
#9193 = AXIS2_PLACEMENT_3D ( 'NONE', #717, #3869, #17615 ) ;
#9194 = CARTESIAN_POINT ( 'NONE',  ( 15.60497028854143764, -26.39208911975253002, -225.8550158017044112 ) ) ;
#9195 = CARTESIAN_POINT ( 'NONE',  ( -9.250876228778270871, 9.538614635316015722, -227.1332118982684563 ) ) ;
#9196 = CARTESIAN_POINT ( 'NONE',  ( -8.005900519654911562, 11.01772743098285545, -228.7074549843708269 ) ) ;
#9197 = ORIENTED_EDGE ( 'NONE', *, *, #3764, .F. ) ;
#9198 = CARTESIAN_POINT ( 'NONE',  ( -8.966714183099560032, 19.05224306381768073, -234.0879867025980445 ) ) ;
#9199 = CARTESIAN_POINT ( 'NONE',  ( -7.786003226018990198, -12.23758553950863082, -224.1954257758910671 ) ) ;
#9200 = DIRECTION ( 'NONE',  ( 0.000000000000000000, 0.000000000000000000, -1.000000000000000000 ) ) ;
#9201 = DIRECTION ( 'NONE',  ( 1.000000000000000000, 0.000000000000000000, 0.000000000000000000 ) ) ;
#9202 = EDGE_CURVE ( 'NONE', #7309, #3391, #8008, .T. ) ;
#9203 = CARTESIAN_POINT ( 'NONE',  ( -10.84997096467605182, 25.01800101807719301, -232.4518260228253155 ) ) ;
#9204 = CARTESIAN_POINT ( 'NONE',  ( 4.150966869518468272, -13.66845483776041092, -221.7292245539943565 ) ) ;
#9205 = DIRECTION ( 'NONE',  ( 0.000000000000000000, 0.000000000000000000, -1.000000000000000000 ) ) ;
#9206 = CARTESIAN_POINT ( 'NONE',  ( -17.39699619235753048, 15.64332637722790054, -216.0406373264262641 ) ) ;
#9207 = CARTESIAN_POINT ( 'NONE',  ( 13.17424634425744046, 10.51488364724239588, -221.4616598107521099 ) ) ;
#9208 = CARTESIAN_POINT ( 'NONE',  ( -16.58369694688956741, 24.75758513462668375, -230.3405478298966784 ) ) ;
#9209 = DIRECTION ( 'NONE',  ( 1.000000000000000000, 0.000000000000000000, 0.000000000000000000 ) ) ;
#9210 = CARTESIAN_POINT ( 'NONE',  ( -18.09994298044773942, 1.383435435878707320, -215.7801353739235708 ) ) ;
#9211 = CARTESIAN_POINT ( 'NONE',  ( -11.04629350503636864, -16.47921676447750983, -219.6257371594006145 ) ) ;
#9212 = VERTEX_POINT ( 'NONE', #19049 ) ;
#9213 =( GEOMETRIC_REPRESENTATION_CONTEXT ( 3 ) GLOBAL_UNCERTAINTY_ASSIGNED_CONTEXT ( ( #7862 ) ) GLOBAL_UNIT_ASSIGNED_CONTEXT ( ( #6764, #15434, #6532 ) ) REPRESENTATION_CONTEXT ( 'NONE', 'WORKASPACE' ) );
#9214 = CARTESIAN_POINT ( 'NONE',  ( -7.250603130619442283, 20.89725557392719324, -217.7893896917081520 ) ) ;
#9215 = CARTESIAN_POINT ( 'NONE',  ( -8.316505849089994129, 18.84563905716333210, -217.0138378867507640 ) ) ;
#9216 = CARTESIAN_POINT ( 'NONE',  ( -13.44241955326339166, 15.88952131657459965, -217.2587743382015901 ) ) ;
#9217 = CARTESIAN_POINT ( 'NONE',  ( -10.71434429704389046, -13.39337408441371124, -228.3296939239235428 ) ) ;
#9218 = DIRECTION ( 'NONE',  ( 0.000000000000000000, 0.000000000000000000, 1.000000000000000000 ) ) ;
#9219 = ORIENTED_EDGE ( 'NONE', *, *, #2358, .F. ) ;
#9220 = CARTESIAN_POINT ( 'NONE',  ( -20.43618815875133521, 1.403378831510147196, -232.9646741665398224 ) ) ;
#9221 = CARTESIAN_POINT ( 'NONE',  ( 6.477082923917054202, -23.79794467951758108, -219.1375485160026813 ) ) ;
#9222 = CARTESIAN_POINT ( 'NONE',  ( 15.85665641241444668, 18.24713744004561988, -217.7195292979064902 ) ) ;
#9223 = CARTESIAN_POINT ( 'NONE',  ( 5.343558017910363667, 26.29639771561252459, -218.1010331760174665 ) ) ;
#9224 = UNCERTAINTY_MEASURE_WITH_UNIT (LENGTH_MEASURE( 1.000000000000000082E-05 ), #16556, 'distance_accuracy_value', 'NONE');
#9225 = AXIS2_PLACEMENT_3D ( 'NONE', #17756, #5918, #9088 ) ;
#9226 = CARTESIAN_POINT ( 'NONE',  ( -25.48569860171343748, 4.299098795181173216, -219.7804659532078801 ) ) ;
#9227 = CARTESIAN_POINT ( 'NONE',  ( 16.11883106748507188, 21.48229216499086291, -233.4985352728212433 ) ) ;
#9228 = EDGE_CURVE ( 'NONE', #18886, #10528, #4757, .T. ) ;
#9229 = CARTESIAN_POINT ( 'NONE',  ( 15.89706143421296147, 10.57416387607782227, -218.3862415393350318 ) ) ;
#9230 = CARTESIAN_POINT ( 'NONE',  ( 13.66960652149700728, 1.853972107162461080, -222.6386165551958811 ) ) ;
#9231 = CARTESIAN_POINT ( 'NONE',  ( -19.50907964299920039, -17.77536300509877876, -217.8007844881196320 ) ) ;
#9232 = CARTESIAN_POINT ( 'NONE',  ( 6.166782020495575445, -26.61202787628535660, -217.6604608484729795 ) ) ;
#9233 = CARTESIAN_POINT ( 'NONE',  ( -21.94776718874820176, -0.4748437386657589632, -216.1214812709574176 ) ) ;
#9234 = CARTESIAN_POINT ( 'NONE',  ( 0.000000000000000000, 23.00000000000000000, -24.99999999999999289 ) ) ;
#9235 = CARTESIAN_POINT ( 'NONE',  ( -26.12939716039095117, 11.33146045174629357, -233.1192402782019997 ) ) ;
#9236 = CARTESIAN_POINT ( 'NONE',  ( -17.04360437375341419, -3.174793268193519591, -228.4680687138289841 ) ) ;
#9237 = CARTESIAN_POINT ( 'NONE',  ( -14.94667331530454213, 6.325011500478772142, -230.0242139990887154 ) ) ;
#9238 = CARTESIAN_POINT ( 'NONE',  ( 16.10596270516584028, 24.75152718569329835, -228.9330127594856492 ) ) ;
#9239 = CARTESIAN_POINT ( 'NONE',  ( 16.49020573214642837, 22.44566021525517741, -224.7841662740084701 ) ) ;
#9240 = ORIENTED_EDGE ( 'NONE', *, *, #8330, .F. ) ;
#9241 = CARTESIAN_POINT ( 'NONE',  ( 17.10065829945946092, -7.211672327051211084, -215.1948405133616404 ) ) ;
#9242 = CARTESIAN_POINT ( 'NONE',  ( 15.05360126642391450, 1.481754003466396963, -222.9454997252120734 ) ) ;
#9243 = CARTESIAN_POINT ( 'NONE',  ( 3.044038000507106378, 30.22621415828681180, -231.1553244844465382 ) ) ;
#9244 = CARTESIAN_POINT ( 'NONE',  ( -19.18087294808806931, 21.32275554655070593, -230.8558978902391061 ) ) ;
#9245 = CARTESIAN_POINT ( 'NONE',  ( -13.08346052978740914, -7.620079078745922274, -220.3923444982454498 ) ) ;
#9246 = CARTESIAN_POINT ( 'NONE',  ( -15.48255455842386219, 10.01793346089237069, -233.1197357361336913 ) ) ;
#9247 = CARTESIAN_POINT ( 'NONE',  ( 7.677656142228014957, -12.40805626191516353, 93.00000000000000000 ) ) ;
#9248 = CARTESIAN_POINT ( 'NONE',  ( 28.22932473237819551, -8.039268142081398949, -226.6539694142420558 ) ) ;
#9249 = CARTESIAN_POINT ( 'NONE',  ( 1.833772325875588027, 13.50593961039006707, -219.8748197804281119 ) ) ;
#9250 = CARTESIAN_POINT ( 'NONE',  ( 14.81258087342262364, 2.398747990731791013, -230.9000679928271040 ) ) ;
#9251 = CARTESIAN_POINT ( 'NONE',  ( 17.28149325064817887, -1.074788064772476792, -229.5315781944399305 ) ) ;
#9252 = CARTESIAN_POINT ( 'NONE',  ( 4.389496648589924277, 14.47660514356954131, -220.6151178996808540 ) ) ;
#9253 = CARTESIAN_POINT ( 'NONE',  ( -14.31049420963804586, -8.435107166214018903, -218.7432863707801403 ) ) ;
#9254 = ORIENTED_EDGE ( 'NONE', *, *, #4400, .T. ) ;
#9255 = CARTESIAN_POINT ( 'NONE',  ( -7.834600152078401436, 27.83486203824852012, -220.1209588485844222 ) ) ;
#9256 = CARTESIAN_POINT ( 'NONE',  ( -1.632242579688942596, -13.62074943359385415, -221.1585305289511041 ) ) ;
#9257 = CARTESIAN_POINT ( 'NONE',  ( 4.559463107227270662, 13.27337529356814017, -226.9596205199204633 ) ) ;
#9258 = CARTESIAN_POINT ( 'NONE',  ( 22.25403255790844881, -22.02690323431350450, -229.4561893391075671 ) ) ;
#9259 = CARTESIAN_POINT ( 'NONE',  ( 0.000000000000000000, -23.00000000000000000, 75.00000000000000000 ) ) ;
#9260 = ADVANCED_FACE ( 'NONE', ( #4074 ), #15801, .T. ) ;
#9261 = CARTESIAN_POINT ( 'NONE',  ( -9.988594796049140356, 11.34066464990972811, -226.6453149279956563 ) ) ;
#9262 =( NAMED_UNIT ( * ) PLANE_ANGLE_UNIT ( ) SI_UNIT ( $, .RADIAN. ) );
#9263 = CARTESIAN_POINT ( 'NONE',  ( 26.38334502096500245, -3.352420239867627494, -217.3603908026431384 ) ) ;
#9264 = CARTESIAN_POINT ( 'NONE',  ( 15.50648685944955218, 24.16641006378193168, -224.4827813270165393 ) ) ;
#9265 = CARTESIAN_POINT ( 'NONE',  ( -26.38808873681881906, 13.30696350521622939, -225.1492950792419663 ) ) ;
#9266 = CARTESIAN_POINT ( 'NONE',  ( 14.98418162551161714, 4.450317369940187895, -227.9894155827521161 ) ) ;
#9267 = CARTESIAN_POINT ( 'NONE',  ( -20.83288780491947279, -19.75659621676223665, -225.4831129403879117 ) ) ;
#9268 = CARTESIAN_POINT ( 'NONE',  ( 25.30941179858102430, 8.661697827793627624, -216.7530520919057722 ) ) ;
#9269 = CARTESIAN_POINT ( 'NONE',  ( 0.000000000000000000, 0.000000000000000000, -77.51594804401857175 ) ) ;
#9270 = CARTESIAN_POINT ( 'NONE',  ( -15.15102066082706678, -13.26725641419114510, -214.8414790003043322 ) ) ;
#9271 = CARTESIAN_POINT ( 'NONE',  ( 3.378648530876271039, 26.08525450992624428, -218.4319906442508454 ) ) ;
#9272 = CARTESIAN_POINT ( 'NONE',  ( 16.21758812354607215, 4.665393561625732488, -232.5634757513959983 ) ) ;
#9273 = CARTESIAN_POINT ( 'NONE',  ( -6.804439720554941395, 15.25609613835249156, -218.7834354895107651 ) ) ;
#9274 = CARTESIAN_POINT ( 'NONE',  ( -5.568057711815838751, 28.69723585065299076, -232.1518503103610271 ) ) ;
#9275 = CARTESIAN_POINT ( 'NONE',  ( 18.69835413980967687, -1.262199651413310031, -230.6153330080101966 ) ) ;
#9276 = CARTESIAN_POINT ( 'NONE',  ( 3.940243381406264511, -15.52098910442465041, -222.4744391328516144 ) ) ;
#9277 = ORIENTED_EDGE ( 'NONE', *, *, #21485, .T. ) ;
#9278 = CARTESIAN_POINT ( 'NONE',  ( 10.46316887740464985, -17.92901728017801233, -232.6108895528913081 ) ) ;
#9279 = CARTESIAN_POINT ( 'NONE',  ( 0.000000000000000000, 0.000000000000000000, 90.00000000000000000 ) ) ;
#9280 = CARTESIAN_POINT ( 'NONE',  ( 21.39553407250273054, 8.453402029343234148, -217.9531594780983141 ) ) ;
#9281 = CARTESIAN_POINT ( 'NONE',  ( 29.17814965709308694, -1.309718763918959139, -225.2029557489520926 ) ) ;
#9282 = CARTESIAN_POINT ( 'NONE',  ( -16.76449091996730090, -6.021196472930381738, -231.5810252088758432 ) ) ;
#9283 = CARTESIAN_POINT ( 'NONE',  ( -1.608171596096409806, -16.77465153034988887, -217.4618546331240054 ) ) ;
#9284 = CARTESIAN_POINT ( 'NONE',  ( 7.042184411928968935, 23.28260216771182556, -230.5707103145148267 ) ) ;
#9285 = CARTESIAN_POINT ( 'NONE',  ( -24.79170285622992509, 4.551775110860766915, -234.5907228154019322 ) ) ;
#9286 = CARTESIAN_POINT ( 'NONE',  ( -18.09776816382430908, 23.50806826204562583, -229.9568677523880638 ) ) ;
#9287 = CARTESIAN_POINT ( 'NONE',  ( 1.030230143518703345, 18.27887886751213387, -229.5791973322770616 ) ) ;
#9288 = CARTESIAN_POINT ( 'NONE',  ( 15.12095272344708263, -0.3261452966805281073, -219.6280520283587805 ) ) ;
#9289 = ORIENTED_EDGE ( 'NONE', *, *, #1436, .T. ) ;
#9290 = ORIENTED_EDGE ( 'NONE', *, *, #2672, .F. ) ;
#9291 = CARTESIAN_POINT ( 'NONE',  ( 12.96449997971774870, 8.285709878278680662, -230.9518598506670628 ) ) ;
#9292 = CARTESIAN_POINT ( 'NONE',  ( -15.07599795178976443, 12.40109266655585429, -218.9921934537110815 ) ) ;
#9293 = CARTESIAN_POINT ( 'NONE',  ( 15.87399429023076003, -1.683916961781461552, -230.8621029165058758 ) ) ;
#9294 = CARTESIAN_POINT ( 'NONE',  ( -5.693514143275418604, -18.22526881224050754, -218.3451910747569968 ) ) ;
#9295 = CYLINDRICAL_SURFACE ( 'NONE', #18764, 20.99999999999999645 ) ;
#9296 = CARTESIAN_POINT ( 'NONE',  ( -20.99999999999999645, 0.000000000000000000, 69.99999999999998579 ) ) ;
#9297 = CARTESIAN_POINT ( 'NONE',  ( 17.19674704922021391, 23.07334190050143974, -228.8256488842130238 ) ) ;
#9298 = CARTESIAN_POINT ( 'NONE',  ( 14.68060984531904012, -6.704174034294832829, -225.1581031080203559 ) ) ;
#9299 = CARTESIAN_POINT ( 'NONE',  ( -14.06164063153489252, 2.050767714179807744, -227.2881998904968270 ) ) ;
#9300 = ADVANCED_FACE ( 'NONE', ( #11061 ), #4042, .T. ) ;
#9301 = CIRCLE ( 'NONE', #4249, 3.000000000000002665 ) ;
#9302 = CARTESIAN_POINT ( 'NONE',  ( 6.741123954526870854, -14.00899218320067341, -219.0418835583997179 ) ) ;
#9303 = CARTESIAN_POINT ( 'NONE',  ( 2.837900457371055563, 25.11342719071438978, -232.9871906064174709 ) ) ;
#9304 = CARTESIAN_POINT ( 'NONE',  ( -17.94782256308196366, 19.07396065564992682, -232.7143578890335220 ) ) ;
#9305 = ORIENTED_EDGE ( 'NONE', *, *, #12993, .T. ) ;
#9306 = CARTESIAN_POINT ( 'NONE',  ( -15.66530208164916260, 23.23467148471576849, -218.1250122661128046 ) ) ;
#9307 = CARTESIAN_POINT ( 'NONE',  ( -11.24961133108761935, -10.18645864713539950, -228.7780882195199013 ) ) ;
#9308 = DIRECTION ( 'NONE',  ( 0.000000000000000000, 0.000000000000000000, -1.000000000000000000 ) ) ;
#9309 = CARTESIAN_POINT ( 'NONE',  ( 2.100000000000000089, 0.000000000000000000, -75.00000000000000000 ) ) ;
#9310 = CARTESIAN_POINT ( 'NONE',  ( -3.326157069579807946, 13.92020081821418565, -220.5733722327383930 ) ) ;
#9311 = CARTESIAN_POINT ( 'NONE',  ( 3.737871636182809265, -14.23896033977216113, -229.0757302894822942 ) ) ;
#9312 = CARTESIAN_POINT ( 'NONE',  ( 14.50031142556784580, -1.551246135476861188, -222.4318553185507028 ) ) ;
#9313 = CARTESIAN_POINT ( 'NONE',  ( -24.24202834850560606, 19.05981756344202438, -226.6980666352953335 ) ) ;
#9314 = CARTESIAN_POINT ( 'NONE',  ( -22.10934047915441170, 0.9940043559354162506, -215.0000000000000000 ) ) ;
#9315 = CARTESIAN_POINT ( 'NONE',  ( -2.043230952238195286, 23.63069326910348877, -232.6835180461029040 ) ) ;
#9316 = AXIS2_PLACEMENT_3D ( 'NONE', #980, #7855, #21557 ) ;
#9317 = CARTESIAN_POINT ( 'NONE',  ( 0.000000000000000000, 23.00000000000006040, -30.00000000000000000 ) ) ;
#9318 = CARTESIAN_POINT ( 'NONE',  ( 15.04029996350473830, 7.457450192165341107, -220.5007084872782173 ) ) ;
#9319 = CARTESIAN_POINT ( 'NONE',  ( -13.63268120803286720, -13.08481847960132249, -219.9337478264210404 ) ) ;
#9320 = ORIENTED_EDGE ( 'NONE', *, *, #22019, .F. ) ;
#9321 = CARTESIAN_POINT ( 'NONE',  ( 2.893760225568064115, 14.39521026618305477, -227.6654023557511550 ) ) ;
#9322 = CARTESIAN_POINT ( 'NONE',  ( -13.41250421226414069, 17.27419134292087577, -217.6844171132545966 ) ) ;
#9323 = CARTESIAN_POINT ( 'NONE',  ( -19.01002492504315811, 19.85266905124972681, -219.0021410556803687 ) ) ;
#9324 = CARTESIAN_POINT ( 'NONE',  ( -21.61315260466662380, -9.974349528768403417, -231.2583083768228960 ) ) ;
#9325 = DIRECTION ( 'NONE',  ( 0.000000000000000000, 0.000000000000000000, -1.000000000000000000 ) ) ;
#9326 = ORIENTED_EDGE ( 'NONE', *, *, #9377, .T. ) ;
#9327 = CARTESIAN_POINT ( 'NONE',  ( -14.70651859537745487, 4.211702956367679107, -230.0357207626005334 ) ) ;
#9328 = CARTESIAN_POINT ( 'NONE',  ( 8.129749879387842881, -22.89596468334109147, -230.6606593278197295 ) ) ;
#9329 = CARTESIAN_POINT ( 'NONE',  ( 16.64225601860865211, 1.926018578292457928, -220.2177910260893725 ) ) ;
#9330 = CARTESIAN_POINT ( 'NONE',  ( -3.855805549595750392, 26.68244055262801950, -232.4569730455296508 ) ) ;
#9331 = DIRECTION ( 'NONE',  ( 1.000000000000000000, 0.000000000000000000, 0.000000000000000000 ) ) ;
#9332 = CARTESIAN_POINT ( 'NONE',  ( -16.29666348338687953, 2.994680995215331709, -221.2421885839926006 ) ) ;
#9333 = CARTESIAN_POINT ( 'NONE',  ( 17.81160404892403193, 9.939217752910943560, -216.9646549374535311 ) ) ;
#9334 = CARTESIAN_POINT ( 'NONE',  ( 23.04897566969193079, 17.95862962700741861, -223.6438515760422661 ) ) ;
#9335 = CARTESIAN_POINT ( 'NONE',  ( 22.00000000000000000, 2.694222958124177598E-15, -224.9999999999999716 ) ) ;
#9336 = CARTESIAN_POINT ( 'NONE',  ( -8.491902988188710921, -10.37035003683405066, -223.9502466269643435 ) ) ;
#9337 = CARTESIAN_POINT ( 'NONE',  ( 3.342529885312644833, -17.78621320651278737, -216.7788622297345853 ) ) ;
#9338 = CARTESIAN_POINT ( 'NONE',  ( -22.44874942423953357, -5.036274748608448704, -8.663716403940144417 ) ) ;
#9339 = ADVANCED_FACE ( 'NONE', ( #21170 ), #7690, .F. ) ;
#9340 = DIRECTION ( 'NONE',  ( 1.000000000000000000, 0.000000000000000000, 0.000000000000000000 ) ) ;
#9341 = CARTESIAN_POINT ( 'NONE',  ( -7.834600152078401436, 27.83486203824852012, -220.1209588485844222 ) ) ;
#9342 = CARTESIAN_POINT ( 'NONE',  ( 27.25858960103340323, -9.764658377823966617, -217.2703135185301448 ) ) ;
#9343 = CARTESIAN_POINT ( 'NONE',  ( 17.00614511541963836, -1.958782916976874233, -219.4638360731791806 ) ) ;
#9344 = CARTESIAN_POINT ( 'NONE',  ( 13.20340559785743828, 9.575208899273587093, -218.1210831379648312 ) ) ;
#9345 = CARTESIAN_POINT ( 'NONE',  ( 11.73428189025226942, 12.46434742632455084, -228.1539301014595083 ) ) ;
#9346 = ORIENTED_EDGE ( 'NONE', *, *, #7888, .T. ) ;
#9347 = CARTESIAN_POINT ( 'NONE',  ( 24.73665505496147432, -17.48642391317526190, -218.9253764065177847 ) ) ;
#9348 = CARTESIAN_POINT ( 'NONE',  ( 10.42862217565707894, 10.07717698332843170, 92.99999999999998579 ) ) ;
#9349 = CARTESIAN_POINT ( 'NONE',  ( 3.744112528862662881, 31.76296354843916703, -227.8872370379487506 ) ) ;
#9350 = CARTESIAN_POINT ( 'NONE',  ( -10.83439284573031536, 18.36737820296253432, -234.3014274143859836 ) ) ;
#9351 = CARTESIAN_POINT ( 'NONE',  ( -12.96708845633950347, -3.368725568741437026, -223.5528514750533873 ) ) ;
#9352 = CARTESIAN_POINT ( 'NONE',  ( -22.11084984981285118, 10.96048252433489623, -216.6117774006995376 ) ) ;
#9353 = DIRECTION ( 'NONE',  ( 4.845403715540889009E-30, -6.938893903907222461E-16, -1.000000000000000000 ) ) ;
#9354 = CARTESIAN_POINT ( 'NONE',  ( 16.06750045776299629, -1.909440863493336860, -220.4398626676318713 ) ) ;
#9355 = CARTESIAN_POINT ( 'NONE',  ( 1.220475224794998370, 29.83033731899746144, -230.4224274340063801 ) ) ;
#9356 = CARTESIAN_POINT ( 'NONE',  ( 18.03440114592047649, 4.755211820135348155, -216.3599228381250157 ) ) ;
#9357 = CARTESIAN_POINT ( 'NONE',  ( -10.65455960636934662, 10.37188583052882862, -219.5197110153079620 ) ) ;
#9358 = CARTESIAN_POINT ( 'NONE',  ( 13.69275646168278371, 8.674223198772375909, -220.8699857572541987 ) ) ;
#9359 = DIRECTION ( 'NONE',  ( -1.000000000000000000, 0.000000000000000000, 0.000000000000000000 ) ) ;
#9360 = ORIENTED_EDGE ( 'NONE', *, *, #4962, .T. ) ;
#9361 = CARTESIAN_POINT ( 'NONE',  ( 5.365126951644291431, 19.60085171667039816, -218.9155869426879519 ) ) ;
#9362 = CARTESIAN_POINT ( 'NONE',  ( -11.20272313682045073, -7.956653478762055087, -225.3025344850567819 ) ) ;
#9363 = CARTESIAN_POINT ( 'NONE',  ( 19.72515656911863147, 14.02277373989196541, -218.0718040828188009 ) ) ;
#9364 = CARTESIAN_POINT ( 'NONE',  ( 2.898952953659251985, -22.97888022809681274, -215.2852275949887826 ) ) ;
#9365 = DIRECTION ( 'NONE',  ( -0.2588190451025213501, 0.000000000000000000, 0.9659258262890680902 ) ) ;
#9366 = CARTESIAN_POINT ( 'NONE',  ( -15.30295614572244922, 9.661125001905515930, -218.8475896279880146 ) ) ;
#9367 = CARTESIAN_POINT ( 'NONE',  ( 23.17317677245511831, -6.950782331930943414, -233.5406539459643227 ) ) ;
#9368 = CARTESIAN_POINT ( 'NONE',  ( 3.182992543297812560, 16.68308636702302650, -221.9272281984358415 ) ) ;
#9369 = CARTESIAN_POINT ( 'NONE',  ( -11.35482716595652875, 11.86850131893102223, -220.6599844941370350 ) ) ;
#9370 = CARTESIAN_POINT ( 'NONE',  ( -18.67456582549428390, 11.07053394491094345, -214.7114755712704550 ) ) ;
#9371 = CARTESIAN_POINT ( 'NONE',  ( -6.532222827695542300, -22.16123078269809099, -233.6760793125601481 ) ) ;
#9372 = CARTESIAN_POINT ( 'NONE',  ( 20.96405783751201213, 6.249056650590980588, -215.6254004080763309 ) ) ;
#9373 = FACE_OUTER_BOUND ( 'NONE', #8722, .T. ) ;
#9374 = CARTESIAN_POINT ( 'NONE',  ( -11.84714279977019125, -8.528511525072332233, -232.0239825124074002 ) ) ;
#9375 = CARTESIAN_POINT ( 'NONE',  ( -4.715783688792956063, 28.29821729825949816, -228.0423900005874600 ) ) ;
#9376 = CARTESIAN_POINT ( 'NONE',  ( 12.81769551943392393, 4.437328497131001193, -221.7762769673541072 ) ) ;
#9377 = EDGE_CURVE ( 'NONE', #930, #945, #20937, .T. ) ;
#9378 = CARTESIAN_POINT ( 'NONE',  ( -13.41250421226414069, 17.27419134292087577, -217.6844171132545966 ) ) ;
#9379 = CARTESIAN_POINT ( 'NONE',  ( 4.914880347045685660, 14.54749271951947698, -232.8668677254037789 ) ) ;
#9380 = CARTESIAN_POINT ( 'NONE',  ( 2.245945009347994237, -28.59251958642781233, -226.9771193766267743 ) ) ;
#9381 = CARTESIAN_POINT ( 'NONE',  ( 1.102456202203287550, -23.13885590315818064, -232.0370787247644557 ) ) ;
#9382 = DIRECTION ( 'NONE',  ( 0.000000000000000000, 0.000000000000000000, -1.000000000000000000 ) ) ;
#9383 = CARTESIAN_POINT ( 'NONE',  ( 25.33562512631297281, 12.25422971834577268, -228.6777356031426791 ) ) ;
#9384 = CARTESIAN_POINT ( 'NONE',  ( 12.70477135646371281, -9.814387909761604689, -230.3443492180780652 ) ) ;
#9385 = CARTESIAN_POINT ( 'NONE',  ( -13.05629324012484282, -10.24599397043673221, -218.7452066004821347 ) ) ;
#9386 = CARTESIAN_POINT ( 'NONE',  ( -15.27057301462635408, -17.00912219741827514, -233.6288396447818627 ) ) ;
#9387 = CARTESIAN_POINT ( 'NONE',  ( 3.191455400233187412, 17.67480163422566619, -220.7055581859663107 ) ) ;
#9388 = LINE ( 'NONE', #5889, #814 ) ;
#9389 = CARTESIAN_POINT ( 'NONE',  ( -11.36937006530106586, 5.486019310970209339, -224.0742584078730033 ) ) ;
#9390 = CARTESIAN_POINT ( 'NONE',  ( 4.543450689403089271, 15.91052110650461771, -218.9437823786444426 ) ) ;
#9391 = CARTESIAN_POINT ( 'NONE',  ( 3.182992543297812560, 16.68308636702302650, -221.9272281984358415 ) ) ;
#9392 = CARTESIAN_POINT ( 'NONE',  ( 13.79223148755288797, -4.990905483784310981, -230.8248327435212559 ) ) ;
#9393 = ORIENTED_EDGE ( 'NONE', *, *, #1509, .F. ) ;
#9394 = CARTESIAN_POINT ( 'NONE',  ( 8.821742718405863215, 10.82866050966069160, -221.4785132813277642 ) ) ;
#9395 = CARTESIAN_POINT ( 'NONE',  ( -12.96364545172611571, 10.77137376900670063, -221.1208843751685720 ) ) ;
#9396 = CARTESIAN_POINT ( 'NONE',  ( 20.96405783751201213, 6.249056650590980588, -215.6254004080763309 ) ) ;
#9397 = CARTESIAN_POINT ( 'NONE',  ( 1.525817648051120967, -14.82969601928396841, -225.8796824437346515 ) ) ;
#9398 = DIRECTION ( 'NONE',  ( -0.000000000000000000, -0.000000000000000000, -1.000000000000000000 ) ) ;
#9399 = VERTEX_POINT ( 'NONE', #15909 ) ;
#9400 = CARTESIAN_POINT ( 'NONE',  ( 3.449504654906655254, 27.59247159270940841, -231.3461799890608859 ) ) ;
#9401 = CARTESIAN_POINT ( 'NONE',  ( 15.64298904066490259, -12.83894575744357880, -230.8789486217465594 ) ) ;
#9402 = DIRECTION ( 'NONE',  ( 0.000000000000000000, -1.000000000000000000, -0.000000000000000000 ) ) ;
#9403 = EDGE_CURVE ( 'NONE', #13305, #8350, #21065, .T. ) ;
#9404 = CARTESIAN_POINT ( 'NONE',  ( -11.07688804854283049, -12.81333559660784971, -232.1241261852632363 ) ) ;
#9405 = CARTESIAN_POINT ( 'NONE',  ( 4.354034006296288339, 14.09944204372416188, -221.2519525881239417 ) ) ;
#9406 = CARTESIAN_POINT ( 'NONE',  ( -0.3984245442872364484, 11.77931270252508789, -223.1826369159892920 ) ) ;
#9407 = ORIENTED_EDGE ( 'NONE', *, *, #5825, .F. ) ;
#9408 = CARTESIAN_POINT ( 'NONE',  ( -16.39453490553961856, 20.24836633112041184, -233.1722131570092245 ) ) ;
#9409 = CARTESIAN_POINT ( 'NONE',  ( 22.35566739451469331, -4.954007294914331894, -217.4158986454943374 ) ) ;
#9410 = CARTESIAN_POINT ( 'NONE',  ( -23.45095836310901660, -8.671879559401306281, -5.022568673106638570 ) ) ;
#9411 = CARTESIAN_POINT ( 'NONE',  ( 0.000000000000000000, 0.000000000000000000, 77.51594804401857175 ) ) ;
#9412 = CARTESIAN_POINT ( 'NONE',  ( -9.171998067665157350, 9.395241133357435714, -226.3428046914542051 ) ) ;
#9413 = CARTESIAN_POINT ( 'NONE',  ( -8.649444225544010934, -13.15555178350489918, -216.8547715670961509 ) ) ;
#9414 = CARTESIAN_POINT ( 'NONE',  ( -1.322875655532295136, 1.500000000000000000, -120.0000000000000142 ) ) ;
#9415 = CARTESIAN_POINT ( 'NONE',  ( -16.39453490553961856, 20.24836633112041184, -233.1722131570092245 ) ) ;
#9416 = AXIS2_PLACEMENT_3D ( 'NONE', #1538, #8416, #1655 ) ;
#9417 = CARTESIAN_POINT ( 'NONE',  ( 20.62963957373278134, 2.372686805184054837, -232.5966151263358483 ) ) ;
#9418 = ADVANCED_FACE ( 'NONE', ( #9373 ), #3687, .T. ) ;
#9419 = CARTESIAN_POINT ( 'NONE',  ( -9.350291727197115321, 27.53754332352430367, -230.1504993026967441 ) ) ;
#9420 = CARTESIAN_POINT ( 'NONE',  ( 13.80743592543072396, -3.637675435010108906E-12, -228.0000000000000568 ) ) ;
#9421 = CARTESIAN_POINT ( 'NONE',  ( 24.96615890023450035, 5.871290975262302148, -218.1661911638112201 ) ) ;
#9422 = CARTESIAN_POINT ( 'NONE',  ( -18.79436262126649027, -19.56097393442729526, -222.1480387859219547 ) ) ;
#9423 = ORIENTED_EDGE ( 'NONE', *, *, #9109, .T. ) ;
#9424 = ADVANCED_FACE ( 'NONE', ( #3851 ), #14558, .F. ) ;
#9425 = CARTESIAN_POINT ( 'NONE',  ( 8.860681144154234801, 27.11956268701432293, -229.8503778060109823 ) ) ;
#9426 = CARTESIAN_POINT ( 'NONE',  ( -17.75632171729475317, 14.45153669854845901, -218.6240360064753929 ) ) ;
#9427 = CARTESIAN_POINT ( 'NONE',  ( -12.39654240422350462, 9.886262337642440556, -219.1620329226848014 ) ) ;
#9428 = CIRCLE ( 'NONE', #4730, 21.00000000000008527 ) ;
#9429 = ORIENTED_EDGE ( 'NONE', *, *, #21404, .F. ) ;
#9430 = CARTESIAN_POINT ( 'NONE',  ( -22.94312929380076937, -2.351969141711130806, -217.0768970835230505 ) ) ;
#9431 = EDGE_CURVE ( 'NONE', #15752, #7178, #2056, .T. ) ;
#9432 = DIRECTION ( 'NONE',  ( 0.000000000000000000, 0.000000000000000000, 1.000000000000000000 ) ) ;
#9433 = ORIENTED_EDGE ( 'NONE', *, *, #8137, .T. ) ;
#9434 = CARTESIAN_POINT ( 'NONE',  ( -16.71711190488355570, 0.6105529133557690002, -230.9511258789794681 ) ) ;
#9435 = CARTESIAN_POINT ( 'NONE',  ( -11.90549671174648694, -23.44716645851259784, -216.8989558407570257 ) ) ;
#9436 = CARTESIAN_POINT ( 'NONE',  ( 13.47977767379887659, 1.040845183112855787, -227.8169118424926296 ) ) ;
#9437 = CARTESIAN_POINT ( 'NONE',  ( 0.2389779871941385414, 16.64595486589868045, -218.1658233406367629 ) ) ;
#9438 = DIRECTION ( 'NONE',  ( 0.000000000000000000, 0.000000000000000000, -1.000000000000000000 ) ) ;
#9439 = CARTESIAN_POINT ( 'NONE',  ( -20.84243560023798736, 1.479777185913828230, -230.9766426496277631 ) ) ;
#9440 = CARTESIAN_POINT ( 'NONE',  ( 9.851209273476317918, 25.48401176094959553, -233.7173763849377792 ) ) ;
#9441 = SHAPE_REPRESENTATION_RELATIONSHIP ( 'NONE' , 'NONE' ,  #1546, #20907 ) ;
#9442 = CIRCLE ( 'NONE', #20570, 23.00000000000008882 ) ;
#9443 = CARTESIAN_POINT ( 'NONE',  ( 15.87442104186276381, 8.674488492264579520, -230.9702037640878416 ) ) ;
#9444 = DIRECTION ( 'NONE',  ( -1.000000000000000000, 0.000000000000000000, 0.000000000000000000 ) ) ;
#9445 = CARTESIAN_POINT ( 'NONE',  ( -25.64743926792790063, -18.08564893845128907, -228.9187414798782925 ) ) ;
#9446 = CARTESIAN_POINT ( 'NONE',  ( -9.625604265899946554, -19.21123364792547505, -233.9327940972253259 ) ) ;
#9447 = APPLICATION_CONTEXT ( 'automotive_design' ) ;
#9448 = FACE_OUTER_BOUND ( 'NONE', #15163, .T. ) ;
#9449 = DIRECTION ( 'NONE',  ( -0.000000000000000000, 0.000000000000000000, -1.000000000000000000 ) ) ;
#9450 = CARTESIAN_POINT ( 'NONE',  ( -1.582540545905128049, 14.52388882916313584, -222.9138157219475147 ) ) ;
#9451 = CARTESIAN_POINT ( 'NONE',  ( 18.12061937846576853, -10.14999073105125227, -235.3098052193838612 ) ) ;
#9452 = CARTESIAN_POINT ( 'NONE',  ( 14.68556740487494849, -6.365102927765655672, -229.6664356779805587 ) ) ;
#9453 = CARTESIAN_POINT ( 'NONE',  ( -13.75208518020500748, 5.661250135068270239, -227.6647651141479685 ) ) ;
#9454 = CARTESIAN_POINT ( 'NONE',  ( 10.70175380652492336, 7.370128018021000038, -224.3479584370086286 ) ) ;
#9455 = CARTESIAN_POINT ( 'NONE',  ( 8.647507700742417924, 16.42978512283924175, -220.3082116258600536 ) ) ;
#9456 = ORIENTED_EDGE ( 'NONE', *, *, #11837, .T. ) ;
#9457 = CARTESIAN_POINT ( 'NONE',  ( 6.889583945421565048, -13.03635046449108081, -231.0237689561592731 ) ) ;
#9458 = CARTESIAN_POINT ( 'NONE',  ( 12.42076324352741956, 7.665070080910708405, 93.00000000000000000 ) ) ;
#9459 = VECTOR ( 'NONE', #17931, 1000.000000000000000 ) ;
#9460 = CARTESIAN_POINT ( 'NONE',  ( -4.845359737286285551, 16.85396349487340117, -233.9229833851842670 ) ) ;
#9461 = CARTESIAN_POINT ( 'NONE',  ( -9.578110717394128670, 23.64032677849093034, -215.7669555765890550 ) ) ;
#9462 = CARTESIAN_POINT ( 'NONE',  ( 23.53402537799887284, -10.66620622184993650, -219.3119847637072439 ) ) ;
#9463 = CARTESIAN_POINT ( 'NONE',  ( -3.003186468682855104, 15.63968344752823469, -231.5301608670590667 ) ) ;
#9464 = CARTESIAN_POINT ( 'NONE',  ( 2.025093002184578772, -14.49031849020018470, 93.00000000000000000 ) ) ;
#9465 = CARTESIAN_POINT ( 'NONE',  ( 0.1866476013601106043, 25.93503619265524307, -233.5574764272258790 ) ) ;
#9466 = CARTESIAN_POINT ( 'NONE',  ( 17.98589043827631428, 2.945998030785370592, -233.4030907785035538 ) ) ;
#9467 = CARTESIAN_POINT ( 'NONE',  ( -9.151299407007059017, 9.196974979111923076, -223.9483834032048719 ) ) ;
#9468 = CARTESIAN_POINT ( 'NONE',  ( 15.42212722119060864, 5.401662248084913465, -220.8333402320903645 ) ) ;
#9469 = TOROIDAL_SURFACE ( 'NONE', #13778, 22.63401512838748175, 3.000000000000002665 ) ;
#9470 = VECTOR ( 'NONE', #10774, 1000.000000000000000 ) ;
#9471 = CARTESIAN_POINT ( 'NONE',  ( -21.94776718874820176, -0.4748437386657589632, -216.1214812709574176 ) ) ;
#9472 = CARTESIAN_POINT ( 'NONE',  ( -2.129100187576105530, 26.11057959790866789, -231.5939360033278547 ) ) ;
#9473 = CARTESIAN_POINT ( 'NONE',  ( -10.11868820210310282, -13.51996935893276053, -218.1704188629865371 ) ) ;
#9474 = CARTESIAN_POINT ( 'NONE',  ( 24.42567939027770407, 10.22651298688739097, -219.4562066833365748 ) ) ;
#9475 = CARTESIAN_POINT ( 'NONE',  ( -7.732225105831920686, -12.76821222370703346, -228.2562058524068220 ) ) ;
#9476 = CARTESIAN_POINT ( 'NONE',  ( 20.12875910279714020, 1.792218354162522953, -222.5869962921167655 ) ) ;
#9477 = CARTESIAN_POINT ( 'NONE',  ( -13.97943781666340790, 5.798109546139844639, -228.2992319913466019 ) ) ;
#9478 =( LENGTH_UNIT ( ) NAMED_UNIT ( * ) SI_UNIT ( .MILLI., .METRE. ) );
#9479 = CARTESIAN_POINT ( 'NONE',  ( 12.75766869239441803, -12.84633107758633663, -232.0853690516983079 ) ) ;
#9480 = CARTESIAN_POINT ( 'NONE',  ( 8.686008240521225332, 26.11221116136006515, -227.6539570933143466 ) ) ;
#9481 = CARTESIAN_POINT ( 'NONE',  ( -14.94667331530454213, 6.325011500478772142, -230.0242139990887154 ) ) ;
#9482 = CARTESIAN_POINT ( 'NONE',  ( -25.32262741784088078, 2.623212696197013472, -234.6011982779809841 ) ) ;
#9483 = CARTESIAN_POINT ( 'NONE',  ( -17.95722789764597849, -8.907256384892455969, -219.4045086951509518 ) ) ;
#9484 = CARTESIAN_POINT ( 'NONE',  ( 25.41781277602550304, 19.49958712797920057, -223.1230538376805441 ) ) ;
#9485 = VECTOR ( 'NONE', #11457, 1000.000000000000000 ) ;
#9486 = CYLINDRICAL_SURFACE ( 'NONE', #6225, 21.50000000000001066 ) ;
#9487 = CARTESIAN_POINT ( 'NONE',  ( -15.30224200789663946, -6.308083384910589508, -216.9633489813582514 ) ) ;
#9488 = CARTESIAN_POINT ( 'NONE',  ( 3.312424284731937618, 15.29837714273186045, -229.5209971419123747 ) ) ;
#9489 = CARTESIAN_POINT ( 'NONE',  ( 17.66525298603349370, 4.919957226727790456, -233.3736646485340032 ) ) ;
#9490 = CARTESIAN_POINT ( 'NONE',  ( -6.127117917506272882, 18.94558806480136681, -232.9763641438055117 ) ) ;
#9491 = CARTESIAN_POINT ( 'NONE',  ( 19.66122710937851537, 22.83208755991274330, -220.0578523118790883 ) ) ;
#9492 = VERTEX_POINT ( 'NONE', #2493 ) ;
#9493 = CARTESIAN_POINT ( 'NONE',  ( -5.077014288276974874, -29.41487918302398796, -226.0100937268998962 ) ) ;
#9494 = EDGE_CURVE ( 'NONE', #6212, #7309, #16233, .T. ) ;
#9495 = CARTESIAN_POINT ( 'NONE',  ( -1.097449620509919788, -25.21235133823365260, -218.6697740411501059 ) ) ;
#9496 = CARTESIAN_POINT ( 'NONE',  ( 20.34032485158648029, 2.741617426884598530, -217.9827731991294968 ) ) ;
#9497 = CARTESIAN_POINT ( 'NONE',  ( 20.38902395782249144, -18.95772103455488633, -230.9098670703349967 ) ) ;
#9498 = CARTESIAN_POINT ( 'NONE',  ( 13.45252989138277400, -0.3779036657139918098, -224.7462000225944792 ) ) ;
#9499 = CARTESIAN_POINT ( 'NONE',  ( -20.83683780809167629, -19.66850649927503625, -219.7460615899071570 ) ) ;
#9500 = CARTESIAN_POINT ( 'NONE',  ( 8.686008240521225332, 26.11221116136006515, -227.6539570933143466 ) ) ;
#9501 = DIRECTION ( 'NONE',  ( -0.9940043559354330149, -0.1093404791528966163, -6.737719923507020479E-14 ) ) ;
#9502 = CARTESIAN_POINT ( 'NONE',  ( 16.55609572527610851, 2.729108819536508967, -230.5704679660131831 ) ) ;
#9503 = VECTOR ( 'NONE', #16942, 1000.000000000000000 ) ;
#9504 = CARTESIAN_POINT ( 'NONE',  ( 5.623554730548537606, 15.65270319720736225, -231.3185741195121068 ) ) ;
#9505 = CARTESIAN_POINT ( 'NONE',  ( -3.015877970456246615, 27.27456613555083464, -227.6995284396757313 ) ) ;
#9506 = CARTESIAN_POINT ( 'NONE',  ( 17.11616244378571494, -1.720737510755655064, -232.0394440302203236 ) ) ;
#9507 = ORIENTED_EDGE ( 'NONE', *, *, #9879, .F. ) ;
#9508 = CARTESIAN_POINT ( 'NONE',  ( 23.21336156720804667, 12.57464006230432574, -232.9346648124233070 ) ) ;
#9509 = CARTESIAN_POINT ( 'NONE',  ( -23.77327857871830830, 11.53128597905896768, -221.0855018166512025 ) ) ;
#9510 = CARTESIAN_POINT ( 'NONE',  ( -25.19195624009214640, 10.50676406307063182, -220.0954552869889937 ) ) ;
#9511 = CARTESIAN_POINT ( 'NONE',  ( -1.434166139689934338, -16.90223958437590213, -219.9603817157532433 ) ) ;
#9512 = LINE ( 'NONE', #14470, #6407 ) ;
#9513 = DIRECTION ( 'NONE',  ( 0.000000000000000000, 0.000000000000000000, -1.000000000000000000 ) ) ;
#9514 = CARTESIAN_POINT ( 'NONE',  ( 14.68783945462866924, 9.535285537539673228, -219.4694094309942045 ) ) ;
#9515 = CARTESIAN_POINT ( 'NONE',  ( 13.81930941494936782, -14.31252807618095879, -218.6132940872857375 ) ) ;
#9516 = DIRECTION ( 'NONE',  ( 0.000000000000000000, 0.000000000000000000, -1.000000000000000000 ) ) ;
#9517 = CARTESIAN_POINT ( 'NONE',  ( -1.778254167844783851, -12.78790610364390012, -225.9413532495922254 ) ) ;
#9518 = SHAPE_DEFINITION_REPRESENTATION ( #8339, #8462 ) ;
#9519 = CARTESIAN_POINT ( 'NONE',  ( -1.881996891245037995, 28.05344686410985489, -218.6379207300106202 ) ) ;
#9520 = CIRCLE ( 'NONE', #22091, 19.63401512838747820 ) ;
#9521 = CARTESIAN_POINT ( 'NONE',  ( 4.719925043692215993, 22.16918918211828782, -214.6883144083888908 ) ) ;
#9522 = VERTEX_POINT ( 'NONE', #2275 ) ;
#9523 = CARTESIAN_POINT ( 'NONE',  ( -7.189383125363055349, 14.28512618638020548, -231.7475838278701303 ) ) ;
#9524 = CARTESIAN_POINT ( 'NONE',  ( 26.42472234358771033, -2.855770380922216134, -231.8949512018254211 ) ) ;
#9525 = COLOUR_RGB ( '', 0.09019608, 0.27058824, 0.51372549) ;
#9526 = CARTESIAN_POINT ( 'NONE',  ( -24.60661961089613925, -4.459629237831038928, -8.974440426817473337 ) ) ;
#9527 = CARTESIAN_POINT ( 'NONE',  ( 0.000000000000000000, 0.000000000000000000, 95.00000000000000000 ) ) ;
#9528 = CARTESIAN_POINT ( 'NONE',  ( -12.90983082593748676, 14.84936372681532823, -233.8009687022269532 ) ) ;
#9529 = CARTESIAN_POINT ( 'NONE',  ( -21.38010734112553024, -21.14131910627544997, -218.4623475309535365 ) ) ;
#9530 = CARTESIAN_POINT ( 'NONE',  ( 15.05686526350529775, -5.555778903407086133, -220.1433349335996468 ) ) ;
#9531 = CARTESIAN_POINT ( 'NONE',  ( -26.74045434827795020, 12.41518252455047744, -220.4617428697642652 ) ) ;
#9532 = CARTESIAN_POINT ( 'NONE',  ( -12.45629340980802269, 5.675423426979704367, -220.8874502847910719 ) ) ;
#9533 = CARTESIAN_POINT ( 'NONE',  ( 4.936777854427027989, 27.97379167488809060, -227.0886654730259124 ) ) ;
#9534 = DIRECTION ( 'NONE',  ( -1.000000000000000000, 0.000000000000000000, 0.000000000000000000 ) ) ;
#9535 = CARTESIAN_POINT ( 'NONE',  ( -11.78887577478644566, 1.715692547334320084, -224.3106172711415525 ) ) ;
#9536 = CARTESIAN_POINT ( 'NONE',  ( -7.149118023545313783, -16.86598457999096823, -220.1902049135764514 ) ) ;
#9537 = ADVANCED_FACE ( 'NONE', ( #7362 ), #8382, .F. ) ;
#9538 = ORIENTED_EDGE ( 'NONE', *, *, #14886, .T. ) ;
#9539 = CARTESIAN_POINT ( 'NONE',  ( 8.379126514044342500, 15.76264856365358646, -232.1787896114811360 ) ) ;
#9540 = CARTESIAN_POINT ( 'NONE',  ( -2.917590128672695293, 18.81591489065672818, -216.3635620530855022 ) ) ;
#9541 = CARTESIAN_POINT ( 'NONE',  ( -17.19162585816985001, -4.675655174483583032, -230.6997921109560821 ) ) ;
#9542 = DIRECTION ( 'NONE',  ( 0.000000000000000000, -1.000000000000000000, 0.000000000000000000 ) ) ;
#9543 = VECTOR ( 'NONE', #15764, 1000.000000000000000 ) ;
#9544 = ORIENTED_EDGE ( 'NONE', *, *, #13072, .T. ) ;
#9545 =( GEOMETRIC_REPRESENTATION_CONTEXT ( 3 ) GLOBAL_UNCERTAINTY_ASSIGNED_CONTEXT ( ( #7426 ) ) GLOBAL_UNIT_ASSIGNED_CONTEXT ( ( #20271, #20610, #11746 ) ) REPRESENTATION_CONTEXT ( 'NONE', 'WORKASPACE' ) );
#9546 = CARTESIAN_POINT ( 'NONE',  ( 21.83031488337932657, -1.542591969257240070, -231.3901500139511427 ) ) ;
#9547 = CARTESIAN_POINT ( 'NONE',  ( -5.472810246302690196, -26.30400724048815420, -218.4657170016378416 ) ) ;
#9548 = CARTESIAN_POINT ( 'NONE',  ( 25.69300549816939494, 5.947472783069708946, -230.6131061331718115 ) ) ;
#9549 = CARTESIAN_POINT ( 'NONE',  ( -1.249406995060579062, 25.48934319316224162, -216.9406480707515072 ) ) ;
#9550 = DIRECTION ( 'NONE',  ( -0.000000000000000000, -0.000000000000000000, -1.000000000000000000 ) ) ;
#9551 = ADVANCED_FACE ( 'NONE', ( #379 ), #7468, .T. ) ;
#9552 = CARTESIAN_POINT ( 'NONE',  ( -16.40443871513620522, 4.023423476741658789, -228.9829044427089002 ) ) ;
#9553 = CARTESIAN_POINT ( 'NONE',  ( 8.730612144237051453, 13.93563980088501886, -217.1627566045470132 ) ) ;
#9554 = CARTESIAN_POINT ( 'NONE',  ( 0.000000000000000000, 0.000000000000000000, 75.34729635533385306 ) ) ;
#9555 = CARTESIAN_POINT ( 'NONE',  ( 19.72515656911863147, 14.02277373989196541, -218.0718040828188009 ) ) ;
#9556 = DIRECTION ( 'NONE',  ( -1.000000000000000000, 0.000000000000000000, 0.000000000000000000 ) ) ;
#9557 = CARTESIAN_POINT ( 'NONE',  ( 25.61231557635624156, -8.129803667132245337, -228.3450084804328242 ) ) ;
#9558 = CARTESIAN_POINT ( 'NONE',  ( -17.21167111787709914, -1.850592482912338799, -230.8442569545952665 ) ) ;
#9559 = AXIS2_PLACEMENT_3D ( 'NONE', #22088, #3283, #15355 ) ;
#9560 = DIRECTION ( 'NONE',  ( -1.000000000000000000, 0.000000000000000000, 0.000000000000000000 ) ) ;
#9561 = FACE_OUTER_BOUND ( 'NONE', #16075, .T. ) ;
#9562 = CARTESIAN_POINT ( 'NONE',  ( -5.861205904341304951, 14.21969934012253312, -219.3213214613830644 ) ) ;
#9563 = CARTESIAN_POINT ( 'NONE',  ( 26.97873870420736253, -17.71910932852193454, -225.8965020979516964 ) ) ;
#9564 = CARTESIAN_POINT ( 'NONE',  ( 23.36729170583618398, -5.500043712341283531, -232.1593072787115375 ) ) ;
#9565 = CARTESIAN_POINT ( 'NONE',  ( -28.31595744342370580, 5.786754998807587924, -229.0820962600229223 ) ) ;
#9566 = CARTESIAN_POINT ( 'NONE',  ( 14.69879291197755222, 10.86005690695417236, -216.7815908316746913 ) ) ;
#9567 = CARTESIAN_POINT ( 'NONE',  ( 11.16964468591631920, 25.71443501674299981, -224.7497461878887464 ) ) ;
#9568 = ORIENTED_EDGE ( 'NONE', *, *, #12948, .F. ) ;
#9569 = CARTESIAN_POINT ( 'NONE',  ( 5.701450259358237460, -28.73672391946437088, -229.2085834618566196 ) ) ;
#9570 = CARTESIAN_POINT ( 'NONE',  ( 20.58703255433590940, 0.4816031003617209372, -231.9427175861361263 ) ) ;
#9571 = CARTESIAN_POINT ( 'NONE',  ( -4.334570222994868161, 11.62786715207288601, -222.6396919303362267 ) ) ;
#9572 = CARTESIAN_POINT ( 'NONE',  ( -8.329232059016652201, 11.81357365351366617, -230.1839637212758021 ) ) ;
#9573 = CARTESIAN_POINT ( 'NONE',  ( 14.36131679319511001, -8.144601358551431858, -221.7207256223857144 ) ) ;
#9574 = CARTESIAN_POINT ( 'NONE',  ( -2.208416658185406334, 29.10348627872611615, -219.8480645685746424 ) ) ;
#9575 = CARTESIAN_POINT ( 'NONE',  ( 9.635142796197660786, -10.84906991693322453, 93.00000000000001421 ) ) ;
#9576 = CIRCLE ( 'NONE', #21778, 21.63401512838748175 ) ;
#9577 = CARTESIAN_POINT ( 'NONE',  ( 2.469769522101480597, 18.85781121334172639, -215.5372409425634430 ) ) ;
#9578 = CARTESIAN_POINT ( 'NONE',  ( 14.17826651990317188, -1.167225063855702683, -222.4240311848849387 ) ) ;
#9579 = CARTESIAN_POINT ( 'NONE',  ( -15.58461825850822180, 18.91734573546571951, -233.7691177939990723 ) ) ;
#9580 = CARTESIAN_POINT ( 'NONE',  ( 15.89706143421296147, 10.57416387607782227, -218.3862415393350318 ) ) ;
#9581 = CARTESIAN_POINT ( 'NONE',  ( 1.820119372073704112, 23.17972341190215246, -230.7270437017659503 ) ) ;
#9582 = CARTESIAN_POINT ( 'NONE',  ( -27.06419889410506485, -1.187659473326917237, -217.6367138431444630 ) ) ;
#9583 = VERTEX_POINT ( 'NONE', #700 ) ;
#9584 = CARTESIAN_POINT ( 'NONE',  ( 16.49020573214642837, 22.44566021525517741, -224.7841662740084701 ) ) ;
#9585 = CARTESIAN_POINT ( 'NONE',  ( -20.11874861854083463, -21.11755179634840474, -229.7504124090357323 ) ) ;
#9586 = CARTESIAN_POINT ( 'NONE',  ( 11.57669841200422134, 10.63052136557218574, -228.9489978335593889 ) ) ;
#9587 = CARTESIAN_POINT ( 'NONE',  ( -0.2114165566986584699, -18.43750818655219703, -233.9360633499430833 ) ) ;
#9588 = VECTOR ( 'NONE', #18026, 1000.000000000000000 ) ;
#9589 = DIRECTION ( 'NONE',  ( 0.000000000000000000, 0.000000000000000000, 1.000000000000000000 ) ) ;
#9590 = CARTESIAN_POINT ( 'NONE',  ( -17.39737143130126285, 7.531548707695031375, -232.0788227848755696 ) ) ;
#9591 = CARTESIAN_POINT ( 'NONE',  ( 10.52067862919218832, -10.34113464825721351, -228.4460540958991714 ) ) ;
#9592 = CARTESIAN_POINT ( 'NONE',  ( 7.067550969709256670, 17.75197616922148569, -219.3387126207321955 ) ) ;
#9593 = CARTESIAN_POINT ( 'NONE',  ( -20.57288920227272655, 16.51351902378409520, -230.8484733908063333 ) ) ;
#9594 = CARTESIAN_POINT ( 'NONE',  ( -31.84745724608465522, 5.474219582435353004, -224.7210333253351564 ) ) ;
#9595 = CARTESIAN_POINT ( 'NONE',  ( -26.02538399328502905, -8.003917019953526335, -222.3553134616452098 ) ) ;
#9596 = CARTESIAN_POINT ( 'NONE',  ( 12.48419387172699579, 6.663456953110941328, -219.2717027540951165 ) ) ;
#9597 = CARTESIAN_POINT ( 'NONE',  ( 0.000000000000000000, 0.000000000000000000, -30.00000000000000000 ) ) ;
#9598 = CARTESIAN_POINT ( 'NONE',  ( -14.30218759248275084, -10.01744029472290620, -234.2423117832250341 ) ) ;
#9599 = CARTESIAN_POINT ( 'NONE',  ( 8.674175678922351196, 20.85307874897338110, -216.6688793998777101 ) ) ;
#9600 = ADVANCED_FACE ( 'NONE', ( #14337 ), #19508, .F. ) ;
#9601 = CARTESIAN_POINT ( 'NONE',  ( 21.77183241683778547, 12.04504704525620085, -233.6005549158834640 ) ) ;
#9602 = CARTESIAN_POINT ( 'NONE',  ( -10.65640919150578192, 23.79238421564942740, -218.1088542024188826 ) ) ;
#9603 = CARTESIAN_POINT ( 'NONE',  ( 19.97628502126439187, 24.50819884991013708, -224.8824979922784735 ) ) ;
#9604 = CARTESIAN_POINT ( 'NONE',  ( 3.323726671003152777, -15.99176757603385823, -228.1400570273458186 ) ) ;
#9605 = CARTESIAN_POINT ( 'NONE',  ( -6.454554286546707154, -27.99704349260872149, -227.4356265632874852 ) ) ;
#9606 = CARTESIAN_POINT ( 'NONE',  ( 14.80394259695730064, 1.224172658189580432, -225.4564070658925061 ) ) ;
#9607 = CARTESIAN_POINT ( 'NONE',  ( 21.53087031351596892, -21.03550532031109555, -227.1077645633325233 ) ) ;
#9608 = CARTESIAN_POINT ( 'NONE',  ( 15.12095272344708263, -0.3261452966805281073, -219.6280520283587805 ) ) ;
#9609 = CARTESIAN_POINT ( 'NONE',  ( -11.20272313682045073, -7.956653478762055087, -225.3025344850567819 ) ) ;
#9610 = CARTESIAN_POINT ( 'NONE',  ( 3.198229568054530070, 16.42319727383711481, -222.3960047798183552 ) ) ;
#9611 = LINE ( 'NONE', #16580, #7760 ) ;
#9612 = CARTESIAN_POINT ( 'NONE',  ( -20.05025075566126702, 1.207204931470905018, -215.1628017022767949 ) ) ;
#9613 = CARTESIAN_POINT ( 'NONE',  ( 4.354034006296288339, 14.09944204372416188, -221.2519525881239417 ) ) ;
#9614 = CARTESIAN_POINT ( 'NONE',  ( 1.296323513242173542, 20.09034598902932345, -230.5712631353794961 ) ) ;
#9615 = CARTESIAN_POINT ( 'NONE',  ( 14.31773767102621875, -28.01644431351170894, -220.7875045263454865 ) ) ;
#9616 = CARTESIAN_POINT ( 'NONE',  ( 27.79746884017060538, 13.63637251724950339, -226.5788410723774575 ) ) ;
#9617 = CARTESIAN_POINT ( 'NONE',  ( -17.65560862077320081, 21.92186454631220371, -221.3776075196718693 ) ) ;
#9618 = CARTESIAN_POINT ( 'NONE',  ( -20.84243560023798736, 1.479777185913828230, -230.9766426496277631 ) ) ;
#9619 = CARTESIAN_POINT ( 'NONE',  ( -7.086613078029399659, -28.17108726511417771, -223.6412629831645233 ) ) ;
#9620 = DIRECTION ( 'NONE',  ( 0.000000000000000000, 0.000000000000000000, -1.000000000000000000 ) ) ;
#9621 = CARTESIAN_POINT ( 'NONE',  ( -4.100000000000000533, 5.021051876504148371E-16, -126.0000000000000284 ) ) ;
#9622 = CARTESIAN_POINT ( 'NONE',  ( 17.99029889091409018, 9.613712288440757092, -232.0298403238024036 ) ) ;
#9623 = CARTESIAN_POINT ( 'NONE',  ( 19.77988345122896163, -10.57228134044703793, -230.8608254296808866 ) ) ;
#9624 = EDGE_CURVE ( 'NONE', #5879, #13000, #5757, .T. ) ;
#9625 = FACE_OUTER_BOUND ( 'NONE', #7896, .T. ) ;
#9626 = CARTESIAN_POINT ( 'NONE',  ( -11.06377138986482933, -15.30386857868810857, -217.0411070525910873 ) ) ;
#9627 = CARTESIAN_POINT ( 'NONE',  ( 1.773982976645536835, 19.12448993322812285, -233.2315972735944172 ) ) ;
#9628 = CARTESIAN_POINT ( 'NONE',  ( 4.754245974719506940, 31.05377813473586102, -220.6166503949300193 ) ) ;
#9629 = EDGE_LOOP ( 'NONE', ( #17769, #6893, #20968, #17542 ) ) ;
#9630 = CARTESIAN_POINT ( 'NONE',  ( -22.99617382825321599, 17.18101613848176967, -230.9512687019100099 ) ) ;
#9631 = CARTESIAN_POINT ( 'NONE',  ( -12.96708845633950347, -3.368725568741437026, -223.5528514750533873 ) ) ;
#9632 = CARTESIAN_POINT ( 'NONE',  ( 30.81364357021286793, -2.580535071768633060, -224.0234450364292513 ) ) ;
#9633 = CARTESIAN_POINT ( 'NONE',  ( -20.77601883660645754, 9.867231145063747988, 1.657240493860027586 ) ) ;
#9634 = CARTESIAN_POINT ( 'NONE',  ( -6.474151797443945533, 21.29193859232740138, -215.9573456447696458 ) ) ;
#9635 = CARTESIAN_POINT ( 'NONE',  ( -6.154316005079235374, -31.08134634390615503, -226.4265589226172892 ) ) ;
#9636 = CARTESIAN_POINT ( 'NONE',  ( 18.22947608839760747, -6.525328669204546905, -217.7409786913911205 ) ) ;
#9637 = CARTESIAN_POINT ( 'NONE',  ( -9.749377714296398878, 10.28442384816749922, -229.3722863967025205 ) ) ;
#9638 = CARTESIAN_POINT ( 'NONE',  ( 16.26115440404298340, 3.800605480264513059, -219.2833057824682612 ) ) ;
#9639 = CARTESIAN_POINT ( 'NONE',  ( 5.104697752190542559, 17.18208638613223016, -220.3923334988619445 ) ) ;
#9640 = FACE_OUTER_BOUND ( 'NONE', #15439, .T. ) ;
#9641 = CARTESIAN_POINT ( 'NONE',  ( -21.39667546302236900, 3.687493526428279100, -235.1435990565495047 ) ) ;
#9642 = CARTESIAN_POINT ( 'NONE',  ( -9.770823421170108602, -12.84821564276127503, -225.3905567659999178 ) ) ;
#9643 = ORIENTED_EDGE ( 'NONE', *, *, #1237, .T. ) ;
#9644 = CARTESIAN_POINT ( 'NONE',  ( -10.02095171162140019, 11.02119725306997111, -224.1251327387667516 ) ) ;
#9645 = CARTESIAN_POINT ( 'NONE',  ( 16.55626903245587656, 22.80423546114836952, -218.9884947126587633 ) ) ;
#9646 = CARTESIAN_POINT ( 'NONE',  ( 5.773563157792669820, 21.63217468058455140, -235.0383461317610170 ) ) ;
#9647 = EDGE_LOOP ( 'NONE', ( #3489, #15345, #19634, #19349, #8835, #20221 ) ) ;
#9648 = CARTESIAN_POINT ( 'NONE',  ( 15.91397826126795323, -3.183288324723350549, -218.2846031002558504 ) ) ;
#9649 = DIRECTION ( 'NONE',  ( 0.000000000000000000, 0.000000000000000000, -1.000000000000000000 ) ) ;
#9650 = EDGE_LOOP ( 'NONE', ( #1714, #1082, #11835, #13011 ) ) ;
#9651 = CARTESIAN_POINT ( 'NONE',  ( -23.52999999174766543, 19.39566142560855866, -221.9446938626390704 ) ) ;
#9652 = CARTESIAN_POINT ( 'NONE',  ( -2.927465716848487887, -13.57531311500885352, -224.4053031992201852 ) ) ;
#9653 = DIRECTION ( 'NONE',  ( -0.000000000000000000, -0.000000000000000000, -1.000000000000000000 ) ) ;
#9654 = CARTESIAN_POINT ( 'NONE',  ( 11.67669251569587985, 24.04736029062789981, -218.5856804285192254 ) ) ;
#9655 = CARTESIAN_POINT ( 'NONE',  ( 12.50000000000000355, 0.000000000000000000, -20.00000000000000000 ) ) ;
#9656 = UNCERTAINTY_MEASURE_WITH_UNIT (LENGTH_MEASURE( 1.000000000000000082E-05 ), #18358, 'distance_accuracy_value', 'NONE');
#9657 = CARTESIAN_POINT ( 'NONE',  ( -17.15943377049709184, 17.77880916606822836, -233.2929083076029144 ) ) ;
#9658 = EDGE_CURVE ( 'NONE', #15704, #13423, #21277, .T. ) ;
#9659 = CARTESIAN_POINT ( 'NONE',  ( 24.81668481317358399, 17.11438712655213124, -222.1096362285750274 ) ) ;
#9660 = SURFACE_STYLE_FILL_AREA ( #15065 ) ;
#9661 = CARTESIAN_POINT ( 'NONE',  ( 13.61857686585203275, 0.5573421744009137146, -222.0497554577703170 ) ) ;
#9662 = CARTESIAN_POINT ( 'NONE',  ( 10.55627441269396094, 10.31758739525044888, -223.1990319438957613 ) ) ;
#9663 = DIRECTION ( 'NONE',  ( 0.000000000000000000, 0.000000000000000000, 1.000000000000000000 ) ) ;
#9664 = CARTESIAN_POINT ( 'NONE',  ( 19.77988345122896163, -10.57228134044703793, -230.8608254296808866 ) ) ;
#9665 = CARTESIAN_POINT ( 'NONE',  ( -15.46216926290318305, -2.495270579625169738, -221.2150947962298631 ) ) ;
#9666 = DIRECTION ( 'NONE',  ( -1.000000000000000000, 0.000000000000000000, 0.000000000000000000 ) ) ;
#9667 = FACE_OUTER_BOUND ( 'NONE', #21194, .T. ) ;
#9668 = CARTESIAN_POINT ( 'NONE',  ( -1.316322971969275502, 14.13179993441458215, -224.9782367179667233 ) ) ;
#9669 = CARTESIAN_POINT ( 'NONE',  ( 17.10065829945946092, -7.211672327051211084, -215.1948405133616404 ) ) ;
#9670 = CARTESIAN_POINT ( 'NONE',  ( 13.82188917133564132, -5.740199443570373816, -227.9076376976435654 ) ) ;
#9671 = CARTESIAN_POINT ( 'NONE',  ( -17.43458823433387650, 2.804998135793385750, -231.8077100320880959 ) ) ;
#9672 = CARTESIAN_POINT ( 'NONE',  ( 14.46993441875745390, 0.2699826811589002284, -230.0986938382904157 ) ) ;
#9673 = CARTESIAN_POINT ( 'NONE',  ( 8.961491954973460849, 17.27041174997091844, -219.7661252763212474 ) ) ;
#9674 = ORIENTED_EDGE ( 'NONE', *, *, #6929, .T. ) ;
#9675 = CARTESIAN_POINT ( 'NONE',  ( 0.2144678239183100965, -16.00554277676860693, -220.6792656679080267 ) ) ;
#9676 = CARTESIAN_POINT ( 'NONE',  ( 10.34297350568055052, 10.16397888138328121, 93.00000000000001421 ) ) ;
#9677 = CARTESIAN_POINT ( 'NONE',  ( -17.22166590524039265, 4.587137274468266135, -215.4863060638890033 ) ) ;
#9678 = CARTESIAN_POINT ( 'NONE',  ( 5.501756899793208255, 15.97909684020861043, -233.9380718515096191 ) ) ;
#9679 = CARTESIAN_POINT ( 'NONE',  ( -1.302381543002304687, 18.65968181418110206, -215.1730913991678449 ) ) ;
#9680 = CARTESIAN_POINT ( 'NONE',  ( 13.49585564903807722, -8.492623513249517586, -227.3331091713134811 ) ) ;
#9681 = CARTESIAN_POINT ( 'NONE',  ( 0.2389779871941385414, 16.64595486589868045, -218.1658233406367629 ) ) ;
#9682 = CARTESIAN_POINT ( 'NONE',  ( -15.23434562258889891, -0.4010941804143903222, -220.4743703065900036 ) ) ;
#9683 = CARTESIAN_POINT ( 'NONE',  ( -5.629016366058284149, 14.31889596247328633, -229.4177297515988414 ) ) ;
#9684 = CARTESIAN_POINT ( 'NONE',  ( -28.00010259152825398, 3.831607968041374157, -225.8381323513402208 ) ) ;
#9685 = CARTESIAN_POINT ( 'NONE',  ( -13.83274569775339202, 16.20364235096346661, -234.0851861771356539 ) ) ;
#9686 = CARTESIAN_POINT ( 'NONE',  ( 18.50911814746675788, 15.92944434255054453, -232.0449215596906072 ) ) ;
#9687 = CARTESIAN_POINT ( 'NONE',  ( 3.755404788550845474, 24.96758616565139022, -220.0839658302907935 ) ) ;
#9688 = DIRECTION ( 'NONE',  ( 0.000000000000000000, 0.000000000000000000, -1.000000000000000000 ) ) ;
#9689 = CARTESIAN_POINT ( 'NONE',  ( 11.87550186346493497, 14.27797038184677270, -220.2068243228838185 ) ) ;
#9690 = CARTESIAN_POINT ( 'NONE',  ( -13.88883449434014672, -11.15328429608096172, -217.8357414694029046 ) ) ;
#9691 = CARTESIAN_POINT ( 'NONE',  ( 21.53262694368047647, 11.06794636811408594, -231.8394491640143826 ) ) ;
#9692 = CARTESIAN_POINT ( 'NONE',  ( 2.374937041136545801, -21.24827930241302099, -215.2851479487023312 ) ) ;
#9693 = CARTESIAN_POINT ( 'NONE',  ( -24.63401512838761320, 3.016796777712736283E-15, 77.51594804401857175 ) ) ;
#9694 = CARTESIAN_POINT ( 'NONE',  ( -8.611121136347097860, 17.46802294375265419, -231.5575697815534113 ) ) ;
#9695 = LINE ( 'NONE', #7795, #19957 ) ;
#9696 = CARTESIAN_POINT ( 'NONE',  ( 12.31594623278127720, -7.047777776961618557, -228.0736214755532956 ) ) ;
#9697 = ADVANCED_FACE ( 'NONE', ( #6091 ), #2715, .T. ) ;
#9698 = CARTESIAN_POINT ( 'NONE',  ( 13.25330606581809789, 10.40242132629824034, -230.9170765704288044 ) ) ;
#9699 = CARTESIAN_POINT ( 'NONE',  ( -8.407534899841293097, 16.91942258446019665, -231.3029992963236339 ) ) ;
#9700 = CARTESIAN_POINT ( 'NONE',  ( -15.39319649241581800, 0.3563955590804028795, -232.4397289486159082 ) ) ;
#9701 = CARTESIAN_POINT ( 'NONE',  ( -21.44067990442788840, -11.35877574734454143, -219.4569350636155605 ) ) ;
#9702 = EDGE_CURVE ( 'NONE', #12646, #2355, #7326, .T. ) ;
#9703 = CARTESIAN_POINT ( 'NONE',  ( -24.05551141223569545, 2.266836731622281498, -230.7594878221277384 ) ) ;
#9704 = CARTESIAN_POINT ( 'NONE',  ( 0.000000000000000000, 0.000000000000000000, 77.51594804401857175 ) ) ;
#9705 = CARTESIAN_POINT ( 'NONE',  ( -13.27281469842883688, -16.60017218729922561, -235.3541344917538254 ) ) ;
#9706 = CARTESIAN_POINT ( 'NONE',  ( 18.23116248274160256, 13.99874872632082123, -216.0593560670294835 ) ) ;
#9707 = CARTESIAN_POINT ( 'NONE',  ( 14.00715608756928532, 4.299235856235253728, -230.2440235370780215 ) ) ;
#9708 = CARTESIAN_POINT ( 'NONE',  ( -11.13829636790841704, 14.30978168460582189, -218.6922574227322400 ) ) ;
#9709 = CARTESIAN_POINT ( 'NONE',  ( 4.401501667365108617, 18.53594119471695123, -215.1186850315663150 ) ) ;
#9710 = ORIENTED_EDGE ( 'NONE', *, *, #20798, .T. ) ;
#9711 = CARTESIAN_POINT ( 'NONE',  ( -0.4195811904800660352, -16.41067541138124852, -229.4634529720845819 ) ) ;
#9712 = VERTEX_POINT ( 'NONE', #1258 ) ;
#9713 = CARTESIAN_POINT ( 'NONE',  ( -3.176860551132370425, -19.01962362838126452, -231.5826211182368297 ) ) ;
#9714 = CARTESIAN_POINT ( 'NONE',  ( -12.13692969104051400, -0.3108940857385004697, -222.6170402347994184 ) ) ;
#9715 = CARTESIAN_POINT ( 'NONE',  ( 15.84759643368428428, -7.142586963752317608, -231.1761396821659673 ) ) ;
#9716 = CARTESIAN_POINT ( 'NONE',  ( -17.21167111787709914, -1.850592482912338799, -230.8442569545952665 ) ) ;
#9717 = CARTESIAN_POINT ( 'NONE',  ( -13.88883449434014672, -11.15328429608096172, -217.8357414694029046 ) ) ;
#9718 = CARTESIAN_POINT ( 'NONE',  ( 16.43556216695724004, 8.397919695511960825, -216.7971521583719152 ) ) ;
#9719 = DIRECTION ( 'NONE',  ( -0.000000000000000000, -1.000000000000000000, -0.000000000000000000 ) ) ;
#9720 = CARTESIAN_POINT ( 'NONE',  ( -11.05707385098054729, 9.265475627845670914, -220.9763772784480693 ) ) ;
#9721 = CARTESIAN_POINT ( 'NONE',  ( 1.217121169770782663, 15.31158828575123110, -230.6845728599757308 ) ) ;
#9722 = CARTESIAN_POINT ( 'NONE',  ( 15.74259730902452858, 17.40808440793174583, -232.1327802909178786 ) ) ;
#9723 = CARTESIAN_POINT ( 'NONE',  ( 10.15560415551905749, -12.94826033684588928, -216.3500876866647502 ) ) ;
#9724 = CARTESIAN_POINT ( 'NONE',  ( 12.98364502352995942, 13.67380631913144029, -233.1535077318696096 ) ) ;
#9725 = CARTESIAN_POINT ( 'NONE',  ( -16.51501534778698854, 10.61825396983174485, -230.5082364903317966 ) ) ;
#9726 = CARTESIAN_POINT ( 'NONE',  ( -1.198425787605166715, -24.00698511249634137, -218.1862405767648170 ) ) ;
#9727 = CARTESIAN_POINT ( 'NONE',  ( -24.63401512838747820, 0.000000000000000000, -77.51594804401857175 ) ) ;
#9728 = CARTESIAN_POINT ( 'NONE',  ( -22.00000000000137490, -2.602085213965210642E-15, -216.9999999999999716 ) ) ;
#9729 = CARTESIAN_POINT ( 'NONE',  ( 26.24002132888527328, 11.62331517472360964, -222.5300873157218859 ) ) ;
#9730 = CARTESIAN_POINT ( 'NONE',  ( 10.49228353591056262, -11.88598183233882644, -227.3718921454133124 ) ) ;
#9731 = CARTESIAN_POINT ( 'NONE',  ( -23.00000000000006750, -1.237926774615798086E-16, -10.00000000000000000 ) ) ;
#9732 = CARTESIAN_POINT ( 'NONE',  ( -1.890995374385051608, -13.09686096954197509, -227.5694739903412085 ) ) ;
#9733 = CONTEXT_DEPENDENT_SHAPE_REPRESENTATION ( #19906, #15171 ) ;
#9734 = CARTESIAN_POINT ( 'NONE',  ( -4.104500432947460808, 15.73223271406093460, -218.0734292856946297 ) ) ;
#9735 = ADVANCED_FACE ( 'NONE', ( #19704 ), #16678, .T. ) ;
#9736 = CARTESIAN_POINT ( 'NONE',  ( 3.982203626615636427, 14.63895582687697150, -217.4952312584269123 ) ) ;
#9737 = ORIENTED_EDGE ( 'NONE', *, *, #6454, .F. ) ;
#9738 = CARTESIAN_POINT ( 'NONE',  ( 1.217121169770782663, 15.31158828575123110, -230.6845728599757308 ) ) ;
#9739 = CARTESIAN_POINT ( 'NONE',  ( -29.74115761720981510, -1.844952462305729401, -220.6656484738778943 ) ) ;
#9740 = CARTESIAN_POINT ( 'NONE',  ( -22.96972983264640078, -9.868964564168473785, 1.646689664842678091 ) ) ;
#9741 = PLANE ( 'NONE',  #8063 ) ;
#9742 = CARTESIAN_POINT ( 'NONE',  ( -3.643097910890548796, 22.16888955197135047, -233.9701981029593298 ) ) ;
#9743 = CARTESIAN_POINT ( 'NONE',  ( -5.131528111146875126, -19.01772154664624992, -215.2265844479019563 ) ) ;
#9744 = CARTESIAN_POINT ( 'NONE',  ( 7.486336813247038258, -29.35413437595724773, -221.4114973598149447 ) ) ;
#9745 = CARTESIAN_POINT ( 'NONE',  ( 16.85953475301105442, -7.801609028127129086, -231.9437213283852941 ) ) ;
#9746 = CARTESIAN_POINT ( 'NONE',  ( -29.98527381603928887, 6.316825171121390525, -230.1108345570740994 ) ) ;
#9747 = CARTESIAN_POINT ( 'NONE',  ( 5.466128392039544259, 27.94759090250835243, -223.5617905851570981 ) ) ;
#9748 = CARTESIAN_POINT ( 'NONE',  ( -17.84981083811007707, 0.8485253248287054628, -231.8041300026935119 ) ) ;
#9749 = CARTESIAN_POINT ( 'NONE',  ( -27.12694304224540076, 7.756125161462346540, -217.3817363082233101 ) ) ;
#9750 = CARTESIAN_POINT ( 'NONE',  ( -18.84435272498963343, -14.36455033211084498, -230.7675749430951555 ) ) ;
#9751 = CARTESIAN_POINT ( 'NONE',  ( -15.30295614572244922, 9.661125001905515930, -218.8475896279880146 ) ) ;
#9752 = CARTESIAN_POINT ( 'NONE',  ( 8.175342817246784577, 19.41817470142738244, -216.6818271833384699 ) ) ;
#9753 = CARTESIAN_POINT ( 'NONE',  ( -4.651113456395510326, 27.58151660986499110, -218.3072938287727141 ) ) ;
#9754 = CARTESIAN_POINT ( 'NONE',  ( -28.68324149884075780, -4.473022182960058934, -227.9839418391680681 ) ) ;
#9755 = DIRECTION ( 'NONE',  ( -0.000000000000000000, 0.000000000000000000, -1.000000000000000000 ) ) ;
#9756 = EDGE_LOOP ( 'NONE', ( #18070, #10634, #18294, #164 ) ) ;
#9757 = CARTESIAN_POINT ( 'NONE',  ( -27.90314475660494153, 12.48829126175061077, -223.3300566725355338 ) ) ;
#9758 = CARTESIAN_POINT ( 'NONE',  ( -18.06397433365231819, -19.82544507610489859, -216.4780239895989951 ) ) ;
#9759 = CARTESIAN_POINT ( 'NONE',  ( 15.34286276367735979, 1.557318373440422565, -222.4358706187587416 ) ) ;
#9760 = CARTESIAN_POINT ( 'NONE',  ( 15.91295838535984331, 21.88410254487826379, -230.9583961155862823 ) ) ;
#9761 = DIRECTION ( 'NONE',  ( -1.000000000000000000, 0.000000000000000000, 0.000000000000000000 ) ) ;
#9762 = CARTESIAN_POINT ( 'NONE',  ( 15.05686526350529775, -5.555778903407086133, -220.1433349335996468 ) ) ;
#9763 = CARTESIAN_POINT ( 'NONE',  ( -16.88427011841620029, 9.219900108593305887, -231.9155403335099948 ) ) ;
#9764 = CARTESIAN_POINT ( 'NONE',  ( 15.90795275983908574, 2.546196724714939297, -229.0855319561646297 ) ) ;
#9765 = PRESENTATION_STYLE_ASSIGNMENT (( #16519 ) ) ;
#9766 = VECTOR ( 'NONE', #11305, 1000.000000000000000 ) ;
#9767 = DIRECTION ( 'NONE',  ( 1.000000000000000000, 0.000000000000000000, 0.000000000000000000 ) ) ;
#9768 = CARTESIAN_POINT ( 'NONE',  ( 21.60524407607017849, 3.028118258437591415, -217.8361640396714449 ) ) ;
#9769 = CARTESIAN_POINT ( 'NONE',  ( 0.000000000000000000, 17.50000000000000711, -30.00000000000000000 ) ) ;
#9770 = CARTESIAN_POINT ( 'NONE',  ( 24.34559900986324621, -8.951716371391148286, -220.6604487471163623 ) ) ;
#9771 = CARTESIAN_POINT ( 'NONE',  ( -23.84209965496292227, -7.976777114481962805, -232.1458837748831456 ) ) ;
#9772 = DIRECTION ( 'NONE',  ( -1.000000000000000000, 0.000000000000000000, 0.000000000000000000 ) ) ;
#9773 = AXIS2_PLACEMENT_3D ( 'NONE', #5633, #20280, #21974 ) ;
#9774 = CARTESIAN_POINT ( 'NONE',  ( 0.000000000000000000, 19.79999999999999716, -78.50000000000000000 ) ) ;
#9775 = CARTESIAN_POINT ( 'NONE',  ( -16.96626096607909417, 26.06638125783293347, -227.3272535207661349 ) ) ;
#9776 = CARTESIAN_POINT ( 'NONE',  ( 10.87654225111433526, -5.446269956799608458, -227.9455542281931741 ) ) ;
#9777 = CARTESIAN_POINT ( 'NONE',  ( 16.08921376350389920, -2.840750994787607731, -229.5571464835293796 ) ) ;
#9778 = CARTESIAN_POINT ( 'NONE',  ( -13.93825237094548619, 9.044872709574327985, -220.1275804576921757 ) ) ;
#9779 = CARTESIAN_POINT ( 'NONE',  ( 17.57135037026572277, 0.09191994211922807634, -232.8447871904542410 ) ) ;
#9780 = CARTESIAN_POINT ( 'NONE',  ( 20.59763700141659015, 7.383112456150029423, -232.0722244125682039 ) ) ;
#9781 = CARTESIAN_POINT ( 'NONE',  ( 8.773758653197093693, -22.96626044227292951, -216.4280442219689178 ) ) ;
#9782 = CARTESIAN_POINT ( 'NONE',  ( 21.31262902390056624, 0.4111834581965390645, -232.0572713672585792 ) ) ;
#9783 = CARTESIAN_POINT ( 'NONE',  ( -22.04004491965229207, 12.41871177236473578, -215.2165492276571115 ) ) ;
#9784 = ADVANCED_FACE ( 'NONE', ( #4289 ), #16460, .F. ) ;
#9785 = AXIS2_PLACEMENT_3D ( 'NONE', #18289, #19956, #6014 ) ;
#9786 = CARTESIAN_POINT ( 'NONE',  ( 12.03015173539790617, 23.46358517874481109, -216.0611092640310744 ) ) ;
#9787 = CARTESIAN_POINT ( 'NONE',  ( 4.228809304811371739, 12.93497549386982470, -230.7917784105561907 ) ) ;
#9788 = CARTESIAN_POINT ( 'NONE',  ( 15.74534598441689504, -4.714293076379259873, -220.2687296774407173 ) ) ;
#9789 = CARTESIAN_POINT ( 'NONE',  ( -4.620781219515533778, 16.99182040716223696, -217.1278208835672672 ) ) ;
#9790 = CARTESIAN_POINT ( 'NONE',  ( -25.29098058636142810, 5.014641116111857144, -217.4658967307323110 ) ) ;
#9791 = AXIS2_PLACEMENT_3D ( 'NONE', #17768, #7528, #2221 ) ;
#9792 = CARTESIAN_POINT ( 'NONE',  ( 15.79748369401691122, 19.19631269170049137, -215.0096632418193963 ) ) ;
#9793 = CARTESIAN_POINT ( 'NONE',  ( -13.63002737749749826, 6.315035547785179837, -227.0490028799284516 ) ) ;
#9794 = CARTESIAN_POINT ( 'NONE',  ( -11.02345917017863464, 29.02019856777526741, -223.9475008740665771 ) ) ;
#9795 = CARTESIAN_POINT ( 'NONE',  ( 22.66390650824515873, 11.48342577402021725, -231.3155567808436217 ) ) ;
#9796 = CARTESIAN_POINT ( 'NONE',  ( 7.508136856874425114, 24.19512352541684663, -230.0608033085341617 ) ) ;
#9797 = CARTESIAN_POINT ( 'NONE',  ( 14.90979066288448429, -1.927202206923867234, -222.7790985701595616 ) ) ;
#9798 = DIRECTION ( 'NONE',  ( 1.000000000000000000, 0.000000000000000000, 0.000000000000000000 ) ) ;
#9799 = CARTESIAN_POINT ( 'NONE',  ( -16.64477864544768337, -2.947896226079009807, -219.6737919733007516 ) ) ;
#9800 = AXIS2_PLACEMENT_3D ( 'NONE', #17851, #19190, #12558 ) ;
#9801 = CARTESIAN_POINT ( 'NONE',  ( 10.83706092800007781, 10.12544885278926543, -227.1716144446442343 ) ) ;
#9802 = CARTESIAN_POINT ( 'NONE',  ( -0.3220389361364618397, -21.73025720764451663, -234.5721229173148856 ) ) ;
#9803 = AXIS2_PLACEMENT_3D ( 'NONE', #12905, #4781, #2653 ) ;
#9804 = CARTESIAN_POINT ( 'NONE',  ( 1.526556658859590243E-13, -21.00000000000000000, 75.00000000000000000 ) ) ;
#9805 = VECTOR ( 'NONE', #14870, 1000.000000000000000 ) ;
#9806 = CARTESIAN_POINT ( 'NONE',  ( -14.87932799058895128, 18.71706570923887369, -231.8731726670167745 ) ) ;
#9807 = SURFACE_SIDE_STYLE ('',( #20029 ) ) ;
#9808 = CARTESIAN_POINT ( 'NONE',  ( 7.640685522499278903, -12.22373526560700441, -226.1755943870604710 ) ) ;
#9809 = CARTESIAN_POINT ( 'NONE',  ( 11.44717363687632528, 10.34477785005100969, -220.4550508611108341 ) ) ;
#9810 = CARTESIAN_POINT ( 'NONE',  ( -4.386767007475907754, 14.39570986262862107, -223.2690175027443615 ) ) ;
#9811 = CARTESIAN_POINT ( 'NONE',  ( -28.76901170826145560, 13.32870333992657663, -228.6722616467874616 ) ) ;
#9812 = CARTESIAN_POINT ( 'NONE',  ( -16.08069336251900339, -10.46797077187589231, -230.6200287382480383 ) ) ;
#9813 = ADVANCED_FACE ( 'NONE', ( #6318 ), #17368, .T. ) ;
#9814 = CARTESIAN_POINT ( 'NONE',  ( -22.32700334442577272, 3.978587747811427988, -218.4803616146862453 ) ) ;
#9815 = DIRECTION ( 'NONE',  ( 0.000000000000000000, 0.000000000000000000, -1.000000000000000000 ) ) ;
#9816 = CARTESIAN_POINT ( 'NONE',  ( 23.12216041205843453, 0.2121350054995089496, -232.0572713672589202 ) ) ;
#9817 = CARTESIAN_POINT ( 'NONE',  ( 5.803912621764987456, 13.01725692290267844, -221.8367675400179166 ) ) ;
#9818 = AXIS2_PLACEMENT_3D ( 'NONE', #8244, #11609, #5986 ) ;
#9819 = CARTESIAN_POINT ( 'NONE',  ( -21.18474081038989354, 8.486062504918864491, -230.7949373529753530 ) ) ;
#9820 = VECTOR ( 'NONE', #9449, 1000.000000000000000 ) ;
#9821 = CARTESIAN_POINT ( 'NONE',  ( 5.773563157792669820, 21.63217468058455140, -235.0383461317610170 ) ) ;
#9822 = ADVANCED_FACE ( 'NONE', ( #1035 ), #7909, .T. ) ;
#9823 = CARTESIAN_POINT ( 'NONE',  ( 4.213939275857851108, 16.79797086795582928, -215.8378124706958943 ) ) ;
#9824 = CARTESIAN_POINT ( 'NONE',  ( -11.81612593381754728, -27.26444769731668671, -229.3107067943240338 ) ) ;
#9825 = ORIENTED_EDGE ( 'NONE', *, *, #12429, .F. ) ;
#9826 = CARTESIAN_POINT ( 'NONE',  ( 1.304950495335150507, -16.28913491483048759, -229.3926418476436027 ) ) ;
#9827 = CARTESIAN_POINT ( 'NONE',  ( -9.722597143579921664, 7.159547510896417499, -227.5730737101346222 ) ) ;
#9828 = CARTESIAN_POINT ( 'NONE',  ( 20.98776729843937972, -13.55153944770713359, -217.5092423276211946 ) ) ;
#9829 = CARTESIAN_POINT ( 'NONE',  ( 26.13397685888192257, -0.5417465609251845837, -217.5756777990261526 ) ) ;
#9830 = CARTESIAN_POINT ( 'NONE',  ( -10.11868820210310282, -13.51996935893276053, -218.1704188629865371 ) ) ;
#9831 = CARTESIAN_POINT ( 'NONE',  ( 9.931717191100288389, 12.93133689537362940, -228.8926047089119038 ) ) ;
#9832 = DIRECTION ( 'NONE',  ( 0.1093404791528972547, -0.9940043559354329039, 0.000000000000000000 ) ) ;
#9833 = CARTESIAN_POINT ( 'NONE',  ( -26.47501633019681577, 13.84484755257420119, -230.0154374881822719 ) ) ;
#9834 = CARTESIAN_POINT ( 'NONE',  ( 21.24820809707834357, 20.59746639607275398, -225.8540969741923732 ) ) ;
#9835 = CARTESIAN_POINT ( 'NONE',  ( 10.50530447320976535, 20.19629329636330084, -217.1354359361034767 ) ) ;
#9836 = CARTESIAN_POINT ( 'NONE',  ( 21.24820809707834357, 20.59746639607275398, -225.8540969741923732 ) ) ;
#9837 = CARTESIAN_POINT ( 'NONE',  ( 27.24384134789437439, -15.00887433271272364, -228.9543321217944083 ) ) ;
#9838 = AXIS2_PLACEMENT_3D ( 'NONE', #3449, #3663, #17191 ) ;
#9839 = CARTESIAN_POINT ( 'NONE',  ( 17.23498165643884761, 6.576565757823654934, -216.5785374982484655 ) ) ;
#9840 = CARTESIAN_POINT ( 'NONE',  ( -12.67136363292824086, 22.56975222910433843, -219.0840033572168011 ) ) ;
#9841 = CARTESIAN_POINT ( 'NONE',  ( -1.585416880194127520, 15.28258783379090424, -231.0852564988603319 ) ) ;
#9842 = CARTESIAN_POINT ( 'NONE',  ( -19.65071121466273496, -22.30814805266854606, -225.1308016072272267 ) ) ;
#9843 = CARTESIAN_POINT ( 'NONE',  ( -29.88125065636863198, 4.504452993877526623, -226.2048141718237275 ) ) ;
#9844 = DIRECTION ( 'NONE',  ( 1.000000000000000000, 0.000000000000000000, -0.000000000000000000 ) ) ;
#9845 = CARTESIAN_POINT ( 'NONE',  ( 12.99034161053428349, 11.71468708507361889, -230.9043293568357740 ) ) ;
#9846 = CARTESIAN_POINT ( 'NONE',  ( 7.337960271553932046, -12.57654522398025065, -224.9099165242034530 ) ) ;
#9847 = CARTESIAN_POINT ( 'NONE',  ( -14.94667331530454213, 6.325011500478772142, -230.0242139990887154 ) ) ;
#9848 = CARTESIAN_POINT ( 'NONE',  ( -1.542335193334551491, -19.71915426430242135, -216.1352730594569209 ) ) ;
#9849 = CARTESIAN_POINT ( 'NONE',  ( -16.98287383830707142, 1.584866439881522648, -221.5391863673846444 ) ) ;
#9850 = CARTESIAN_POINT ( 'NONE',  ( -4.424820997438546399, 11.84746159238278373, -221.7815792475208525 ) ) ;
#9851 = VERTEX_POINT ( 'NONE', #14772 ) ;
#9852 = CARTESIAN_POINT ( 'NONE',  ( 2.008896548638861024, 20.64812324442097591, -233.5818019448501843 ) ) ;
#9853 = CARTESIAN_POINT ( 'NONE',  ( -14.76610802599379291, -3.249507257478274180, -230.1617063156812719 ) ) ;
#9854 = DIRECTION ( 'NONE',  ( -1.000000000000000000, 0.000000000000000000, 0.000000000000000000 ) ) ;
#9855 = AXIS2_PLACEMENT_3D ( 'NONE', #21878, #6582, #9969 ) ;
#9856 = CARTESIAN_POINT ( 'NONE',  ( -3.673551555920188783, 29.81207051619892923, -228.8770490300152005 ) ) ;
#9857 = CARTESIAN_POINT ( 'NONE',  ( -11.40836237951390508, -18.42461209671423816, -214.6264694599774430 ) ) ;
#9858 = CARTESIAN_POINT ( 'NONE',  ( 13.36656406724190305, -19.73987914515934960, -233.3798509643240209 ) ) ;
#9859 = CARTESIAN_POINT ( 'NONE',  ( 20.89700225552940793, -4.547446057044195911, -232.3806459760843666 ) ) ;
#9860 = CARTESIAN_POINT ( 'NONE',  ( -15.57505478537380306, 24.84242291948262249, -225.5907943047649837 ) ) ;
#9861 = CARTESIAN_POINT ( 'NONE',  ( 12.94599882983645145, 15.82237817288049442, -219.3332542656393116 ) ) ;
#9862 = DIRECTION ( 'NONE',  ( -1.000000000000000000, 0.000000000000000000, 0.000000000000000000 ) ) ;
#9863 = CARTESIAN_POINT ( 'NONE',  ( -11.05707385098054729, 9.265475627845670914, -220.9763772784480693 ) ) ;
#9864 = CARTESIAN_POINT ( 'NONE',  ( -22.93762879021373280, -16.04239672171475206, -226.2337446402420653 ) ) ;
#9865 = CARTESIAN_POINT ( 'NONE',  ( -15.51982305277792307, 19.76957551617798359, -231.4018974401358832 ) ) ;
#9866 = CARTESIAN_POINT ( 'NONE',  ( 30.60340911705754863, 5.703403611927857497, -225.1938343315648297 ) ) ;
#9867 = CARTESIAN_POINT ( 'NONE',  ( -1.585416880194127520, 15.28258783379090424, -231.0852564988603319 ) ) ;
#9868 = CARTESIAN_POINT ( 'NONE',  ( 24.57161139520042781, -7.530326316930160857, -232.9949629211864419 ) ) ;
#9869 = CARTESIAN_POINT ( 'NONE',  ( -13.12488928717151637, 0.000000000000000000, -105.0000000000000000 ) ) ;
#9870 = ORIENTED_EDGE ( 'NONE', *, *, #20358, .T. ) ;
#9871 = CARTESIAN_POINT ( 'NONE',  ( -16.39453490553961856, 20.24836633112041184, -233.1722131570092245 ) ) ;
#9872 = CARTESIAN_POINT ( 'NONE',  ( -11.81612593381754728, -27.26444769731668671, -229.3107067943240338 ) ) ;
#9873 = CARTESIAN_POINT ( 'NONE',  ( 0.000000000000000000, 0.000000000000000000, -126.0000000000000284 ) ) ;
#9874 = CIRCLE ( 'NONE', #1241, 4.100000000000000533 ) ;
#9875 = CARTESIAN_POINT ( 'NONE',  ( 17.19674704922021391, 23.07334190050143974, -228.8256488842130238 ) ) ;
#9876 = LINE ( 'NONE', #16741, #8775 ) ;
#9877 = CARTESIAN_POINT ( 'NONE',  ( 25.54997870115619207, -2.097555195297153841, -218.7002440566220400 ) ) ;
#9878 = CARTESIAN_POINT ( 'NONE',  ( -13.55591840520136770, 8.363404288414606924, -231.2690188357804857 ) ) ;
#9879 = EDGE_CURVE ( 'NONE', #7880, #8548, #9108, .T. ) ;
#9880 = CARTESIAN_POINT ( 'NONE',  ( -11.01414002179357610, 8.614420160880040811, -226.3770540798392972 ) ) ;
#9881 = CARTESIAN_POINT ( 'NONE',  ( 17.76485367938521875, 4.373152267827974171, -218.8623009891758215 ) ) ;
#9882 = FACE_OUTER_BOUND ( 'NONE', #2414, .T. ) ;
#9883 = CARTESIAN_POINT ( 'NONE',  ( 19.66230024959842382, -2.213945732971099201, -222.9658176208924942 ) ) ;
#9884 = CARTESIAN_POINT ( 'NONE',  ( -14.10849459794400751, -0.2436790717799666162, -223.1085195285415921 ) ) ;
#9885 = CARTESIAN_POINT ( 'NONE',  ( 17.02517607141322031, -4.660589389729973497, -229.0519452290894833 ) ) ;
#9886 = CARTESIAN_POINT ( 'NONE',  ( -18.34948365288241590, -1.907751280579004893, -231.5848060246952116 ) ) ;
#9887 = CARTESIAN_POINT ( 'NONE',  ( 21.30903826138435875, -0.6807850236355832418, -227.9267136575444397 ) ) ;
#9888 = CARTESIAN_POINT ( 'NONE',  ( -20.99999999999999645, 0.000000000000000000, -69.99999999999998579 ) ) ;
#9889 = CARTESIAN_POINT ( 'NONE',  ( 11.21155440434494643, 24.57152134148167733, -221.7155903571010356 ) ) ;
#9890 = CARTESIAN_POINT ( 'NONE',  ( 3.924989892941122438, -14.79802789183876044, -219.9433972157300445 ) ) ;
#9891 = TOROIDAL_SURFACE ( 'NONE', #12418, 22.00000000000000711, 2.999999999999999112 ) ;
#9892 = CARTESIAN_POINT ( 'NONE',  ( 12.73130673999417795, -23.76414828096303467, -217.7386337832039942 ) ) ;
#9893 = MECHANICAL_DESIGN_GEOMETRIC_PRESENTATION_REPRESENTATION (  '', ( #22095 ), #19925 ) ;
#9894 = CARTESIAN_POINT ( 'NONE',  ( -13.70798801564395752, 13.71024986321384809, -218.3360451569033955 ) ) ;
#9895 = CARTESIAN_POINT ( 'NONE',  ( 21.04928763009552384, -0.2309942901367783852, -233.9427286327411366 ) ) ;
#9896 = CARTESIAN_POINT ( 'NONE',  ( 23.74723497152361062, 5.524508269105988134, -217.6012181427065002 ) ) ;
#9897 = VERTEX_POINT ( 'NONE', #6203 ) ;
#9898 = CARTESIAN_POINT ( 'NONE',  ( 5.229904874806564408, -24.29892824652383609, -233.0630010234598046 ) ) ;
#9899 = CARTESIAN_POINT ( 'NONE',  ( -7.743026158993134622, -7.484971844052081380, 92.00000000000000000 ) ) ;
#9900 = CARTESIAN_POINT ( 'NONE',  ( -17.58289524052909414, 0.7988212499981205417, -233.9567931471624149 ) ) ;
#9901 = SHAPE_REPRESENTATION ( 'Soft-Touch Power _ Function Switch', ( #6677 ), #16347 ) ;
#9902 = CARTESIAN_POINT ( 'NONE',  ( 10.35958063030883025, 8.003303894222913328, -225.9303204057916048 ) ) ;
#9903 = CARTESIAN_POINT ( 'NONE',  ( -0.3984245442872364484, 11.77931270252508789, -223.1826369159892920 ) ) ;
#9904 = CARTESIAN_POINT ( 'NONE',  ( 21.28979032490934031, -14.07620925358629727, -230.4022181401844875 ) ) ;
#9905 = CARTESIAN_POINT ( 'NONE',  ( -7.825349071214003693, 24.14595706726266755, -216.5959661901539732 ) ) ;
#9906 = CARTESIAN_POINT ( 'NONE',  ( -15.20262116893801974, 8.038155052917188570, -217.6767387945475036 ) ) ;
#9907 = ADVANCED_FACE ( 'NONE', ( #3044, #14667 ), #21727, .F. ) ;
#9908 = AXIS2_PLACEMENT_3D ( 'NONE', #12017, #12353, #2204 ) ;
#9909 = CARTESIAN_POINT ( 'NONE',  ( 6.523529190399725231, 13.69551997595937465, -217.3678933099786832 ) ) ;
#9910 = STYLED_ITEM ( 'NONE', ( #21965 ), #21655 ) ;
#9911 = CARTESIAN_POINT ( 'NONE',  ( -23.43012680803641956, 15.46310457140252304, -230.0052977649806962 ) ) ;
#9912 = CARTESIAN_POINT ( 'NONE',  ( -9.517741096562200909, 20.63709896626785678, -234.1036702156204967 ) ) ;
#9913 = CARTESIAN_POINT ( 'NONE',  ( -3.593890535426079946, 10.35670734540881455, 92.00000000000001421 ) ) ;
#9914 = CARTESIAN_POINT ( 'NONE',  ( 6.225744896574323839, 14.38227537199079720, -224.8391693295998266 ) ) ;
#9915 = CARTESIAN_POINT ( 'NONE',  ( 16.08921376350389920, -2.840750994787607731, -229.5571464835293796 ) ) ;
#9916 = DIRECTION ( 'NONE',  ( 0.000000000000000000, 0.000000000000000000, 1.000000000000000000 ) ) ;
#9917 = FACE_OUTER_BOUND ( 'NONE', #7634, .T. ) ;
#9918 = CARTESIAN_POINT ( 'NONE',  ( 18.46552355142154411, 5.019711608606525211, -231.5099115070375433 ) ) ;
#9919 = CARTESIAN_POINT ( 'NONE',  ( -19.73058714482073128, -19.33240507441191625, -228.8766180877602494 ) ) ;
#9920 = DIRECTION ( 'NONE',  ( 4.408728476930457445E-15, -1.000000000000000000, 0.000000000000000000 ) ) ;
#9921 = CARTESIAN_POINT ( 'NONE',  ( -4.067324790461362305, 15.10342260507846746, -228.2464404076259257 ) ) ;
#9922 = CARTESIAN_POINT ( 'NONE',  ( 10.05733608402134216, -9.620616164199983444, -224.9449885650552119 ) ) ;
#9923 = CARTESIAN_POINT ( 'NONE',  ( 12.49127101283658803, 6.474961340449192804, -221.2149164507559078 ) ) ;
#9924 = CARTESIAN_POINT ( 'NONE',  ( -7.873497077133136735, 15.44270125396616677, -230.2562282217168672 ) ) ;
#9925 = CARTESIAN_POINT ( 'NONE',  ( -8.328662059352005542, 28.53523473722178139, -221.4280032538016201 ) ) ;
#9926 = ORIENTED_EDGE ( 'NONE', *, *, #17888, .F. ) ;
#9927 = CARTESIAN_POINT ( 'NONE',  ( -16.25683815890624473, -3.869351682469674980, -222.5551530127839044 ) ) ;
#9928 = AXIS2_PLACEMENT_3D ( 'NONE', #7116, #13982, #12282 ) ;
#9929 = CIRCLE ( 'NONE', #12804, 25.00000000000010303 ) ;
#9930 = CARTESIAN_POINT ( 'NONE',  ( -20.84243560023798736, 1.479777185913828230, -230.9766426496277631 ) ) ;
#9931 = DIRECTION ( 'NONE',  ( 0.000000000000000000, 0.000000000000000000, -1.000000000000000000 ) ) ;
#9932 = CARTESIAN_POINT ( 'NONE',  ( -29.78324924674133456, -0.2661018803894699136, -229.0431670511964057 ) ) ;
#9933 = CARTESIAN_POINT ( 'NONE',  ( 11.01659168199870287, 19.17922986229587323, -233.3715978632214387 ) ) ;
#9934 = CARTESIAN_POINT ( 'NONE',  ( -15.82036597035495795, 4.920771916499852239, -223.0095317795067160 ) ) ;
#9935 = CARTESIAN_POINT ( 'NONE',  ( 2.770531592831002143, 22.28948935999365943, -215.1307751200139649 ) ) ;
#9936 = CARTESIAN_POINT ( 'NONE',  ( 22.37138132874926910, 6.723028048925958622, -217.7073806909121743 ) ) ;
#9937 = VECTOR ( 'NONE', #21717, 1000.000000000000000 ) ;
#9938 = EDGE_CURVE ( 'NONE', #9979, #11981, #4056, .T. ) ;
#9939 = VERTEX_POINT ( 'NONE', #19811 ) ;
#9940 = CARTESIAN_POINT ( 'NONE',  ( -19.49800774256867086, -24.03546784425654792, -228.3621204403185061 ) ) ;
#9941 = VERTEX_POINT ( 'NONE', #18036 ) ;
#9942 = CARTESIAN_POINT ( 'NONE',  ( -19.75205891382245227, -22.10994567413457546, -223.7241504221178729 ) ) ;
#9943 = CARTESIAN_POINT ( 'NONE',  ( -29.15345109632842124, 14.07532767497844262, -225.0972140442887621 ) ) ;
#9944 = CARTESIAN_POINT ( 'NONE',  ( 8.818493748348606331, -10.89961555176610375, -227.9481955143288303 ) ) ;
#9945 = CARTESIAN_POINT ( 'NONE',  ( -29.27492217116574480, -1.185422171198730501, -224.8132346143397342 ) ) ;
#9946 = CARTESIAN_POINT ( 'NONE',  ( -14.73155177304599306, -1.817590056890399763, -226.9769936995019748 ) ) ;
#9947 = CARTESIAN_POINT ( 'NONE',  ( 24.49559427486850893, 14.86117239466233642, -230.3058416388274736 ) ) ;
#9948 = AXIS2_PLACEMENT_3D ( 'NONE', #2092, #411, #11312 ) ;
#9949 = DIRECTION ( 'NONE',  ( -1.000000000000000000, 0.000000000000000000, 0.000000000000000000 ) ) ;
#9950 = CARTESIAN_POINT ( 'NONE',  ( -21.95649697515285581, 20.70968357470995258, -226.9638023349746447 ) ) ;
#9951 = CARTESIAN_POINT ( 'NONE',  ( 13.41709597927210496, 19.57823531746157997, -218.2666972400567147 ) ) ;
#9952 = CARTESIAN_POINT ( 'NONE',  ( 8.496844655769807630, 14.66037471857024599, -219.1631158796573118 ) ) ;
#9953 = CARTESIAN_POINT ( 'NONE',  ( 15.50648685944955218, 24.16641006378193168, -224.4827813270165393 ) ) ;
#9954 = CARTESIAN_POINT ( 'NONE',  ( 14.71544223636061410, -24.97731814513734605, -232.6985170686097320 ) ) ;
#9955 = CARTESIAN_POINT ( 'NONE',  ( -9.222253059793434460, 13.27185325399938165, -229.0864811363590547 ) ) ;
#9956 = CARTESIAN_POINT ( 'NONE',  ( -16.71711190488355570, 0.6105529133557690002, -230.9511258789794681 ) ) ;
#9957 = DIRECTION ( 'NONE',  ( 1.000000000000000000, 0.000000000000000000, 0.000000000000000000 ) ) ;
#9958 = CARTESIAN_POINT ( 'NONE',  ( 10.78187269046063435, 10.73871010366167944, -221.9206544238666368 ) ) ;
#9959 = CARTESIAN_POINT ( 'NONE',  ( 11.40994021191102092, -13.94644022156852969, -230.1289083636806936 ) ) ;
#9960 = CARTESIAN_POINT ( 'NONE',  ( -13.37045227479810094, 5.250293981428504786, -224.2914120185227205 ) ) ;
#9961 = CARTESIAN_POINT ( 'NONE',  ( 9.336393807558161839, 27.79372469574263960, -228.5913636680961361 ) ) ;
#9962 = CARTESIAN_POINT ( 'NONE',  ( -18.53787071664277519, -6.556543064843903146, -232.5192140591401824 ) ) ;
#9963 = CARTESIAN_POINT ( 'NONE',  ( -19.67797246974518544, 1.229961341702398681, -219.4743747885323160 ) ) ;
#9964 = CARTESIAN_POINT ( 'NONE',  ( 19.66580438618080251, 15.18147523775131624, -233.5153994334876586 ) ) ;
#9965 = EDGE_LOOP ( 'NONE', ( #21314, #15274, #11175, #16368 ) ) ;
#9966 = CARTESIAN_POINT ( 'NONE',  ( 5.331555957413248059, 27.50712867803999728, -219.0801070358024276 ) ) ;
#9967 = CARTESIAN_POINT ( 'NONE',  ( 23.10971261601581617, -16.35996695089516706, -224.5402406813554421 ) ) ;
#9968 = CARTESIAN_POINT ( 'NONE',  ( 15.07245478799217686, -4.018468087397350175, -231.0118529037252699 ) ) ;
#9969 = DIRECTION ( 'NONE',  ( 1.000000000000000000, 0.000000000000000000, 0.000000000000000000 ) ) ;
#9970 = CARTESIAN_POINT ( 'NONE',  ( -2.934221234790329369, 15.07857928364152222, -230.9558365497803720 ) ) ;
#9971 = CARTESIAN_POINT ( 'NONE',  ( -27.72233273893307981, -16.15685914833838410, -223.8945077613443289 ) ) ;
#9972 = CARTESIAN_POINT ( 'NONE',  ( 6.131461862964278531, -15.14974102410872625, -231.6805438559109973 ) ) ;
#9973 = CARTESIAN_POINT ( 'NONE',  ( 9.104026917753444081, -10.66572815660443041, -221.9193219976906448 ) ) ;
#9974 = CARTESIAN_POINT ( 'NONE',  ( -16.65220264499505376, 11.77543314451157563, -216.3149620944649030 ) ) ;
#9975 = CARTESIAN_POINT ( 'NONE',  ( 9.280831573919673616, 14.67893982993557422, -228.6940810986570796 ) ) ;
#9976 = CARTESIAN_POINT ( 'NONE',  ( -20.43618815875133521, 1.403378831510147196, -232.9646741665398224 ) ) ;
#9977 = CARTESIAN_POINT ( 'NONE',  ( -24.79170285622992509, 4.551775110860766915, -234.5907228154019322 ) ) ;
#9978 = CARTESIAN_POINT ( 'NONE',  ( -14.51900513504577717, -8.991447007532661573, -221.0515111571761793 ) ) ;
#9979 = VERTEX_POINT ( 'NONE', #2604 ) ;
#9980 = CARTESIAN_POINT ( 'NONE',  ( -12.78923236353123727, 15.53885160143439315, -231.8946633672937878 ) ) ;
#9981 = CARTESIAN_POINT ( 'NONE',  ( 21.77183241683778547, 12.04504704525620085, -233.6005549158834640 ) ) ;
#9982 = CARTESIAN_POINT ( 'NONE',  ( -5.629016366058284149, 14.31889596247328633, -229.4177297515988414 ) ) ;
#9983 = ADVANCED_FACE ( 'NONE', ( #14885 ), #9486, .T. ) ;
#9984 = CARTESIAN_POINT ( 'NONE',  ( 13.39541376241636783, -3.462025909069690321, -228.4300562622815391 ) ) ;
#9985 = CARTESIAN_POINT ( 'NONE',  ( -12.50000000000000355, 1.836970198721030378E-15, -20.00000000000000000 ) ) ;
#9986 = VERTEX_POINT ( 'NONE', #4512 ) ;
#9987 = CARTESIAN_POINT ( 'NONE',  ( -15.66530208164916260, 23.23467148471576849, -218.1250122661128046 ) ) ;
#9988 = CARTESIAN_POINT ( 'NONE',  ( -13.00317340065129557, -2.278067296278880161, -219.8118061108488916 ) ) ;
#9989 = DIRECTION ( 'NONE',  ( -0.000000000000000000, -0.000000000000000000, 1.000000000000000000 ) ) ;
#9990 = CARTESIAN_POINT ( 'NONE',  ( 12.58590500897257947, 11.38573988265384607, -230.4867078522624695 ) ) ;
#9991 = CYLINDRICAL_SURFACE ( 'NONE', #17389, 23.00000000000000000 ) ;
#9992 = CARTESIAN_POINT ( 'NONE',  ( 24.05826999138443156, -14.97270453765939102, -220.1026142722873260 ) ) ;
#9993 = CARTESIAN_POINT ( 'NONE',  ( -16.71711190488355570, 0.6105529133557690002, -230.9511258789794681 ) ) ;
#9994 = CARTESIAN_POINT ( 'NONE',  ( -18.41237742040652847, 14.06446039901721790, -216.7469276929859632 ) ) ;
#9995 = CARTESIAN_POINT ( 'NONE',  ( 28.62253243811995418, 3.652502539191337494, -225.4068779441649326 ) ) ;
#9996 = CARTESIAN_POINT ( 'NONE',  ( -0.8337089444836248697, -27.22572500676309559, -220.1932236949194532 ) ) ;
#9997 = CARTESIAN_POINT ( 'NONE',  ( -24.11388480999612938, 6.602120135752692853, -7.517827584289036302 ) ) ;
#9998 = CARTESIAN_POINT ( 'NONE',  ( 18.77064933249684486, -2.992341472042426620, -224.7538226556079337 ) ) ;
#9999 = CARTESIAN_POINT ( 'NONE',  ( 0.000000000000000000, 23.00000000000006040, -69.99999999999998579 ) ) ;
#10000 = CARTESIAN_POINT ( 'NONE',  ( 17.01404819207892061, -3.492736430306117690, -221.2516733069050190 ) ) ;
#10001 = CARTESIAN_POINT ( 'NONE',  ( -14.40111287326894640, -6.123720356435734757, -220.5571602876142094 ) ) ;
#10002 = DIRECTION ( 'NONE',  ( -0.000000000000000000, -0.000000000000000000, 1.000000000000000000 ) ) ;
#10003 = CARTESIAN_POINT ( 'NONE',  ( 24.99999999999999645, 1.360023205165816762E-13, 0.000000000000000000 ) ) ;
#10004 = CARTESIAN_POINT ( 'NONE',  ( 7.951191770265756631, 20.55701948568933091, -231.2149185317973661 ) ) ;
#10005 = CARTESIAN_POINT ( 'NONE',  ( 4.286954182150454429, -15.41507397180808425, -219.0323159710399352 ) ) ;
#10006 = CARTESIAN_POINT ( 'NONE',  ( 19.68037530048075112, -17.97179847169212508, -231.8517058357153076 ) ) ;
#10007 = CARTESIAN_POINT ( 'NONE',  ( -10.32994309255856535, 16.55762392127841665, -218.3313395458419279 ) ) ;
#10008 = CARTESIAN_POINT ( 'NONE',  ( 20.13946171159960841, -0.1427001808266660232, -233.7987036390019853 ) ) ;
#10009 = CARTESIAN_POINT ( 'NONE',  ( 24.52860916307685457, 12.75391509163817361, -221.3604763108436941 ) ) ;
#10010 = CARTESIAN_POINT ( 'NONE',  ( -11.27700245477877772, -16.92453807419676792, -219.4498264308321609 ) ) ;
#10011 = CARTESIAN_POINT ( 'NONE',  ( 10.76794919243112680, -2.946239868469075596, 92.00000000000000000 ) ) ;
#10012 = CARTESIAN_POINT ( 'NONE',  ( -22.61701582078733708, 5.416317966792455252, -214.6955127214549748 ) ) ;
#10013 = VERTEX_POINT ( 'NONE', #2928 ) ;
#10014 = CARTESIAN_POINT ( 'NONE',  ( 9.533850545951205291, 16.09136358716069637, -215.9093469876620475 ) ) ;
#10015 = CARTESIAN_POINT ( 'NONE',  ( 22.40610909459028122, -16.32493987272327018, -222.3848458449739951 ) ) ;
#10016 = CARTESIAN_POINT ( 'NONE',  ( 1.382955251742491898, 16.46353944795171032, -231.7743150979565030 ) ) ;
#10017 = CARTESIAN_POINT ( 'NONE',  ( -17.84981083811007707, 0.8485253248287054628, -231.8041300026935119 ) ) ;
#10018 = VECTOR ( 'NONE', #2190, 1000.000000000000000 ) ;
#10019 = CARTESIAN_POINT ( 'NONE',  ( 17.65694480011521250, 15.62497337860048674, -235.2008064134603273 ) ) ;
#10020 = CARTESIAN_POINT ( 'NONE',  ( -18.91027996815576628, 5.295101183552822555, -231.2253513302548527 ) ) ;
#10021 = PRODUCT_RELATED_PRODUCT_CATEGORY ( 'part', '', ( #18761 ) ) ;
#10022 = CARTESIAN_POINT ( 'NONE',  ( -6.282398543089500187, 12.01615879894893801, -228.5121145169883903 ) ) ;
#10023 = CARTESIAN_POINT ( 'NONE',  ( 7.681243287386652518, 7.547795605678436104, 91.99999999999998579 ) ) ;
#10024 = CARTESIAN_POINT ( 'NONE',  ( 3.281983756374524663, 15.83593597903271721, -223.8697822987047346 ) ) ;
#10025 = CARTESIAN_POINT ( 'NONE',  ( 29.17814965709308694, -1.309718763918959139, -225.2029557489520926 ) ) ;
#10026 = LINE ( 'NONE', #15098, #20672 ) ;
#10027 = CARTESIAN_POINT ( 'NONE',  ( -21.00000000000008171, 0.000000000000000000, 60.00000000000001421 ) ) ;
#10028 = CARTESIAN_POINT ( 'NONE',  ( 19.20300624114736721, 0.6066039755357417462, -231.5046416827383950 ) ) ;
#10029 = CARTESIAN_POINT ( 'NONE',  ( -21.59231333450971135, -13.53975872187591989, -230.0942117760813517 ) ) ;
#10030 = CARTESIAN_POINT ( 'NONE',  ( 19.38184807124233799, 2.462809743167411636, -226.7245352501389846 ) ) ;
#10031 =( BOUNDED_CURVE ( )  B_SPLINE_CURVE ( 3, ( #21949, #1923, #6886, #10480 ),
 .UNSPECIFIED., .F., .F. ) 
 B_SPLINE_CURVE_WITH_KNOTS ( ( 4, 4 ),
 ( 0.000000000000000000, 3.141592653589793116 ),
 .UNSPECIFIED. ) 
 CURVE ( )  GEOMETRIC_REPRESENTATION_ITEM ( )  RATIONAL_B_SPLINE_CURVE ( ( 1.000000000000000000, 0.3333333333333333703, 0.3333333333333333703, 1.000000000000000000 ) ) 
 REPRESENTATION_ITEM ( '' )  );
#10032 = CARTESIAN_POINT ( 'NONE',  ( -11.16203726658389606, 26.27101666727781648, -227.8592829514190612 ) ) ;
#10033 = CARTESIAN_POINT ( 'NONE',  ( 5.380811198380419214, -14.52623441703906160, -221.9013399998540024 ) ) ;
#10034 = CARTESIAN_POINT ( 'NONE',  ( 13.60311248493089131, 7.003372205918751092, -219.1738832909067867 ) ) ;
#10035 = CARTESIAN_POINT ( 'NONE',  ( -9.627017372966443887, 15.60690227900018279, -218.8878023709062859 ) ) ;
#10037 = AXIS2_PLACEMENT_3D ( 'NONE', #4569, #9755, #14721 ) ;
#10036 = CARTESIAN_POINT ( 'NONE',  ( -23.70973587455150522, 20.45398817402440983, -228.9005348699235469 ) ) ;
#10038 = EDGE_LOOP ( 'NONE', ( #6263, #8079, #9240, #13116 ) ) ;
#10039 = CARTESIAN_POINT ( 'NONE',  ( 27.82583766398256486, 0.7543585032809253521, -232.9329547162639358 ) ) ;
#10040 = CARTESIAN_POINT ( 'NONE',  ( 10.66614775643814994, 26.29080367171353672, -230.0818785118670178 ) ) ;
#10041 = CARTESIAN_POINT ( 'NONE',  ( -27.11599398522282911, 10.60460483532474996, -224.7310548435675912 ) ) ;
#10042 = CARTESIAN_POINT ( 'NONE',  ( -16.90857133559978465, -0.4126725064255206687, -221.6276144895144569 ) ) ;
#10043 = CARTESIAN_POINT ( 'NONE',  ( -2.775557561562891351E-14, 0.000000000000000000, -105.0000000000000142 ) ) ;
#10044 = CARTESIAN_POINT ( 'NONE',  ( -30.11338598929818389, -8.317867968210222784, -227.6364879822423006 ) ) ;
#10045 = CARTESIAN_POINT ( 'NONE',  ( 11.64932556965463561, 7.668732705389711413, -229.0406978839571366 ) ) ;
#10046 = CARTESIAN_POINT ( 'NONE',  ( -26.87016840655871874, 6.086699737350822481, -222.9228935003981746 ) ) ;
#10047 = CARTESIAN_POINT ( 'NONE',  ( 1.833772325875588027, 13.50593961039006707, -219.8748197804281119 ) ) ;
#10048 = CARTESIAN_POINT ( 'NONE',  ( 18.55287065739596031, 7.869864349944380777, -232.8430408253643691 ) ) ;
#10049 = CARTESIAN_POINT ( 'NONE',  ( -10.04615645102154886, -9.695712423306433791, -230.4834384258168996 ) ) ;
#10050 = VERTEX_POINT ( 'NONE', #922 ) ;
#10051 = CARTESIAN_POINT ( 'NONE',  ( -14.03072379416114757, -18.13329758221107824, -232.5220584501505812 ) ) ;
#10052 = CARTESIAN_POINT ( 'NONE',  ( -11.79271689233719478, 3.876813423829604144, -228.6816298097564299 ) ) ;
#10053 = CARTESIAN_POINT ( 'NONE',  ( 5.953549895739506326, -12.70069413479034104, -221.3143591192976203 ) ) ;
#10054 = CARTESIAN_POINT ( 'NONE',  ( -3.082945806077231676, 30.69897765966285874, -224.2387254578930822 ) ) ;
#10055 = CARTESIAN_POINT ( 'NONE',  ( 21.04926289057418742, -6.455467962217539934, -215.4677037730695872 ) ) ;
#10056 = CARTESIAN_POINT ( 'NONE',  ( -13.72709560065558421, -5.132649126379569715, -227.9317987811764965 ) ) ;
#10057 = CARTESIAN_POINT ( 'NONE',  ( 14.29768887814754663, 10.87030385293788548, -231.8067013864770161 ) ) ;
#10058 = CARTESIAN_POINT ( 'NONE',  ( -9.403561938624596550, 12.70246821120386471, -220.7484614495429582 ) ) ;
#10059 = CARTESIAN_POINT ( 'NONE',  ( 10.49810582199713416, 9.357428619962972149, -224.5466107281195605 ) ) ;
#10060 = CARTESIAN_POINT ( 'NONE',  ( 12.99034161053428349, 11.71468708507361889, -230.9043293568357740 ) ) ;
#10061 = CARTESIAN_POINT ( 'NONE',  ( 10.98110116949302828, 13.70618071521442971, -230.2797640191687378 ) ) ;
#10062 = CARTESIAN_POINT ( 'NONE',  ( 9.867031390707305505, -6.965612358230354850, -226.9368589251366188 ) ) ;
#10063 = CARTESIAN_POINT ( 'NONE',  ( -2.047892494109819328, 12.88402507277750786, -223.5104301352110951 ) ) ;
#10064 = CARTESIAN_POINT ( 'NONE',  ( -13.10651848559790444, 3.262242204071156948, -224.3513854875720597 ) ) ;
#10065 = EDGE_CURVE ( 'NONE', #20525, #5465, #17023, .T. ) ;
#10066 = CARTESIAN_POINT ( 'NONE',  ( 0.000000000000000000, 0.000000000000000000, -120.0000000000000142 ) ) ;
#10067 = CARTESIAN_POINT ( 'NONE',  ( 8.716925653960343467, -14.61958666771473858, -219.5525962724747444 ) ) ;
#10068 = CARTESIAN_POINT ( 'NONE',  ( -19.74163224554151697, 8.726897413558679872, -232.6665747339030190 ) ) ;
#10069 = CARTESIAN_POINT ( 'NONE',  ( -3.494873682963683059, 27.70407912598904687, -220.5214894769905243 ) ) ;
#10070 = CARTESIAN_POINT ( 'NONE',  ( -15.22366728182010043, -5.552021002219007961, -230.2511309519622671 ) ) ;
#10071 = CARTESIAN_POINT ( 'NONE',  ( -21.48978835671764287, 1.062155088816892468, -219.0000000007146355 ) ) ;
#10072 = CARTESIAN_POINT ( 'NONE',  ( 24.78222556642275620, 17.97262539535998371, -226.6641400693514470 ) ) ;
#10073 = ORIENTED_EDGE ( 'NONE', *, *, #2267, .T. ) ;
#10074 = CARTESIAN_POINT ( 'NONE',  ( 4.883314309504700468, 19.06839645569368358, -217.0171359871271193 ) ) ;
#10075 = CARTESIAN_POINT ( 'NONE',  ( 11.60500945006145024, -11.05507752957471190, -226.0500390094313730 ) ) ;
#10076 = CARTESIAN_POINT ( 'NONE',  ( 17.44158214791148964, -8.186237638883257617, -216.9355394212118995 ) ) ;
#10077 = DIRECTION ( 'NONE',  ( 0.000000000000000000, 0.000000000000000000, -1.000000000000000000 ) ) ;
#10078 = CARTESIAN_POINT ( 'NONE',  ( -1.881996891245037995, 28.05344686410985489, -218.6379207300106202 ) ) ;
#10079 = CARTESIAN_POINT ( 'NONE',  ( -9.664312646807834639, -7.057764824546099547, -227.2890491868971594 ) ) ;
#10080 = CARTESIAN_POINT ( 'NONE',  ( -13.60146639818222702, -25.11808310587244009, -230.9974232610874196 ) ) ;
#10081 = CARTESIAN_POINT ( 'NONE',  ( 21.30961698559626427, -20.48616475849644303, -228.5322376518520002 ) ) ;
#10082 = CARTESIAN_POINT ( 'NONE',  ( -21.75607741976026333, 20.26169853110213381, -228.4128163609909450 ) ) ;
#10083 = CARTESIAN_POINT ( 'NONE',  ( 14.12692363916921146, 20.59586666873830296, -230.0804552526094540 ) ) ;
#10084 = CARTESIAN_POINT ( 'NONE',  ( -23.49379658590067876, 11.46840048879614393, -217.2519070826072323 ) ) ;
#10085 = CARTESIAN_POINT ( 'NONE',  ( -12.45629340980802269, 5.675423426979704367, -220.8874502847910719 ) ) ;
#10086 = CARTESIAN_POINT ( 'NONE',  ( -13.68888474783054399, -8.264665463295720826, -223.0168115903771024 ) ) ;
#10087 = ORIENTED_EDGE ( 'NONE', *, *, #13361, .F. ) ;
#10088 = CARTESIAN_POINT ( 'NONE',  ( -4.490213599459100813, 14.55066867058898694, -222.6488251579668827 ) ) ;
#10089 = CARTESIAN_POINT ( 'NONE',  ( 14.63115627273841923, 9.024791562541032874, -232.5054678133655841 ) ) ;
#10090 = CARTESIAN_POINT ( 'NONE',  ( 10.86206282953156510, 30.27427353967719981, -226.0953027964478110 ) ) ;
#10091 = CARTESIAN_POINT ( 'NONE',  ( 17.44158214791148964, -8.186237638883257617, -216.9355394212118995 ) ) ;
#10092 = CARTESIAN_POINT ( 'NONE',  ( -24.63401512838757768, 0.000000000000000000, -77.51594804401857175 ) ) ;
#10093 = VERTEX_POINT ( 'NONE', #20037 ) ;
#10094 = EDGE_CURVE ( 'NONE', #3236, #12201, #22040, .T. ) ;
#10095 = CARTESIAN_POINT ( 'NONE',  ( -22.11084984981285118, 10.96048252433489623, -216.6117774006995376 ) ) ;
#10096 = CARTESIAN_POINT ( 'NONE',  ( -14.84991717770350661, -12.66914290363892270, -234.6513150936106626 ) ) ;
#10097 = CARTESIAN_POINT ( 'NONE',  ( 0.000000000000000000, 0.000000000000000000, -75.05807060175870049 ) ) ;
#10098 = CARTESIAN_POINT ( 'NONE',  ( 10.55627441269396094, 10.31758739525044888, -223.1990319438957613 ) ) ;
#10099 = LINE ( 'NONE', #11556, #5151 ) ;
#10100 = CARTESIAN_POINT ( 'NONE',  ( 12.13827923251525220, -9.172799829723585319, -229.1860353116090891 ) ) ;
#10101 = PRESENTATION_STYLE_ASSIGNMENT (( #22013 ) ) ;
#10102 = CARTESIAN_POINT ( 'NONE',  ( -27.90314475660494153, 12.48829126175061077, -223.3300566725355338 ) ) ;
#10103 = CARTESIAN_POINT ( 'NONE',  ( 16.20788843645364352, 6.828976201867700269, -231.6689701909764665 ) ) ;
#10104 = CARTESIAN_POINT ( 'NONE',  ( -13.53581065110708970, -26.13331550560631555, -224.9773145811678887 ) ) ;
#10105 = LINE ( 'NONE', #6613, #19527 ) ;
#10106 = ADVANCED_FACE ( 'NONE', ( #18260 ), #2824, .T. ) ;
#10107 = CARTESIAN_POINT ( 'NONE',  ( 14.63113973005795643, 4.926264598692385199, -222.4866305912601945 ) ) ;
#10108 = CARTESIAN_POINT ( 'NONE',  ( 10.49228353591056262, -11.88598183233882644, -227.3718921454133124 ) ) ;
#10109 = CARTESIAN_POINT ( 'NONE',  ( 14.16658675964390923, -1.854297863920779221, -227.3584270016860103 ) ) ;
#10110 = CARTESIAN_POINT ( 'NONE',  ( 20.79630060232303634, -1.171431775223993110, -227.7672307301629075 ) ) ;
#10111 = CARTESIAN_POINT ( 'NONE',  ( 8.162622027327667951, 13.88735946031204094, -224.7165241036068153 ) ) ;
#10112 = CARTESIAN_POINT ( 'NONE',  ( 2.914696262605396715, 19.49933023975583879, -231.6035545612375017 ) ) ;
#10113 = EDGE_CURVE ( 'NONE', #2762, #2965, #10031, .T. ) ;
#10114 = CARTESIAN_POINT ( 'NONE',  ( 9.772444363920737231, -9.146208674228628155, -219.7841758423534486 ) ) ;
#10115 = CARTESIAN_POINT ( 'NONE',  ( 14.18709644517307922, -11.45356969546147496, -232.2178450427173004 ) ) ;
#10116 = VERTEX_POINT ( 'NONE', #18921 ) ;
#10117 = CARTESIAN_POINT ( 'NONE',  ( -11.05032764129755840, 11.65053160594169945, -221.1796278216217218 ) ) ;
#10118 = CARTESIAN_POINT ( 'NONE',  ( 26.91963614581376874, 6.107751173605064920, -232.2246916053503298 ) ) ;
#10119 = CARTESIAN_POINT ( 'NONE',  ( 14.03916608299427082, 11.26328028684000415, -220.2447382113059007 ) ) ;
#10120 = ORIENTED_EDGE ( 'NONE', *, *, #10180, .T. ) ;
#10121 = CARTESIAN_POINT ( 'NONE',  ( -3.614824051224299950, -15.07124992037100064, -223.1721701483932065 ) ) ;
#10122 = CARTESIAN_POINT ( 'NONE',  ( -14.48452571672253342, 0.8583760989383736328, 93.00000000000001421 ) ) ;
#10123 = CARTESIAN_POINT ( 'NONE',  ( -20.02994071726468661, 1.326980477106467271, -234.9527056834518532 ) ) ;
#10124 = ORIENTED_EDGE ( 'NONE', *, *, #21072, .F. ) ;
#10125 = CARTESIAN_POINT ( 'NONE',  ( 18.39533937270110187, 14.26564464607222504, -233.9088367426310242 ) ) ;
#10126 = CARTESIAN_POINT ( 'NONE',  ( 11.72806877847873253, -14.77654346318461975, -220.1368134445341695 ) ) ;
#10127 = CARTESIAN_POINT ( 'NONE',  ( 7.743212835174657194, 11.90778931056080481, -226.0491028376908105 ) ) ;
#10128 = CARTESIAN_POINT ( 'NONE',  ( -12.78558550453068854, 7.693178343823584342, -230.0800953344970878 ) ) ;
#10129 = CARTESIAN_POINT ( 'NONE',  ( 25.12984891811676036, 19.96069634721137476, -226.7154725927711070 ) ) ;
#10130 = CARTESIAN_POINT ( 'NONE',  ( -23.30382222616342247, 9.914163031146200566, -218.5285240371296425 ) ) ;
#10131 = AXIS2_PLACEMENT_3D ( 'NONE', #4491, #17797, #19573 ) ;
#10132 = CARTESIAN_POINT ( 'NONE',  ( -0.9414827276148034496, 23.96885519606619752, -216.4491898092606164 ) ) ;
#10133 = FACE_OUTER_BOUND ( 'NONE', #6623, .T. ) ;
#10134 = CARTESIAN_POINT ( 'NONE',  ( -0.1947256686167265494, -30.94043057420685727, -223.1178397439027492 ) ) ;
#10135 = DIRECTION ( 'NONE',  ( 0.000000000000000000, 0.000000000000000000, -1.000000000000000000 ) ) ;
#10136 = PRODUCT ( 'top housing_top housing', 'top housing_top housing', '', ( #2638 ) ) ;
#10137 = CARTESIAN_POINT ( 'NONE',  ( -18.53787071664277519, -6.556543064843903146, -232.5192140591401824 ) ) ;
#10138 = CARTESIAN_POINT ( 'NONE',  ( -21.85741505224184777, 1.741064654082184582, -235.1654459941842390 ) ) ;
#10139 = CARTESIAN_POINT ( 'NONE',  ( -16.08690871037762449, -24.16943144049835368, -222.8355329163958345 ) ) ;
#10140 = CARTESIAN_POINT ( 'NONE',  ( 25.00000000000000000, 0.000000000000000000, 75.00000000000000000 ) ) ;
#10141 = CIRCLE ( 'NONE', #21250, 16.23205080756887853 ) ;
#10142 = CARTESIAN_POINT ( 'NONE',  ( 5.452943511046377090, -14.64908918772281865, -221.6090591728701611 ) ) ;
#10143 = CARTESIAN_POINT ( 'NONE',  ( 10.25308675723727347, 13.16459519580956972, -229.3963488176951273 ) ) ;
#10144 = CARTESIAN_POINT ( 'NONE',  ( -14.94618804342693075, 22.09718979644185666, -219.6454806548149463 ) ) ;
#10145 = CARTESIAN_POINT ( 'NONE',  ( -17.81561310496929806, 18.25637658208611569, -215.7745954696244439 ) ) ;
#10146 = VERTEX_POINT ( 'NONE', #15227 ) ;
#10147 = CARTESIAN_POINT ( 'NONE',  ( 12.24504971509987072, -1.481354005294047926, -221.9045230856115438 ) ) ;
#10148 = ORIENTED_EDGE ( 'NONE', *, *, #7643, .F. ) ;
#10149 = CARTESIAN_POINT ( 'NONE',  ( 15.33737796850231305, 13.57479350230705428, -232.3313557812109025 ) ) ;
#10150 = CARTESIAN_POINT ( 'NONE',  ( -18.91027996815576628, 5.295101183552822555, -231.2253513302548527 ) ) ;
#10151 = CARTESIAN_POINT ( 'NONE',  ( 29.21307215008108216, 4.139194015751272104, -229.9658791484231699 ) ) ;
#10152 = CIRCLE ( 'NONE', #13020, 23.00000000000008882 ) ;
#10153 = DIRECTION ( 'NONE',  ( 1.224646799147353207E-16, 1.000000000000000000, -0.000000000000000000 ) ) ;
#10154 = CARTESIAN_POINT ( 'NONE',  ( 7.018811797190238622, 13.93862807232938472, -230.2855929063610176 ) ) ;
#10155 = CARTESIAN_POINT ( 'NONE',  ( -23.52458685063474420, 4.195399146287285497, -230.7490123595086970 ) ) ;
#10156 = CARTESIAN_POINT ( 'NONE',  ( -5.566280468132954518, 29.91920859341914962, -222.2705790733167817 ) ) ;
#10157 = CARTESIAN_POINT ( 'NONE',  ( 24.34047711160105720, 17.90454708687460794, -228.1939002122307159 ) ) ;
#10158 = CARTESIAN_POINT ( 'NONE',  ( -5.902345112435694041, -11.50736153130091388, -224.0878888885884805 ) ) ;
#10159 = VECTOR ( 'NONE', #116, 1000.000000000000000 ) ;
#10160 = ORIENTED_EDGE ( 'NONE', *, *, #14391, .F. ) ;
#10161 = CARTESIAN_POINT ( 'NONE',  ( -6.266309075335420253, -15.78290365675015572, -230.2363798222519051 ) ) ;
#10162 = CARTESIAN_POINT ( 'NONE',  ( -17.92628912275201003, -0.6090139417824500523, -215.7724435048976943 ) ) ;
#10163 = CARTESIAN_POINT ( 'NONE',  ( 8.510712203779903007, -27.79691582975998898, -230.5316902582456180 ) ) ;
#10164 = CARTESIAN_POINT ( 'NONE',  ( -3.843007962268670585, 27.94983497691806917, -231.4302614368887703 ) ) ;
#10165 = CARTESIAN_POINT ( 'NONE',  ( 13.42973690470193837, -10.83953015014330035, -233.9990574442320224 ) ) ;
#10166 = CARTESIAN_POINT ( 'NONE',  ( -22.20848920810297855, -2.028924892417935055, -232.4401719831211039 ) ) ;
#10167 = CARTESIAN_POINT ( 'NONE',  ( 21.27834046766391651, 19.84195992785746654, -221.8454931627593965 ) ) ;
#10168 = CARTESIAN_POINT ( 'NONE',  ( 26.00000000000000000, 1.360023205165816762E-13, 10.00000000000000000 ) ) ;
#10169 = CARTESIAN_POINT ( 'NONE',  ( -19.01002492504315811, 19.85266905124972681, -219.0021410556803687 ) ) ;
#10170 = CARTESIAN_POINT ( 'NONE',  ( 12.54860906168727652, 6.077542143275485031, -228.1605930327268368 ) ) ;
#10171 = CARTESIAN_POINT ( 'NONE',  ( 14.31308345469695453, 12.76656023072872159, -231.9445021321040770 ) ) ;
#10172 = CARTESIAN_POINT ( 'NONE',  ( 14.61121792518381390, 23.81825453963186590, -227.9329146581663110 ) ) ;
#10173 = CARTESIAN_POINT ( 'NONE',  ( 5.326148043627311424, -14.37544986528147639, -217.4292808685971750 ) ) ;
#10174 = CARTESIAN_POINT ( 'NONE',  ( -13.14888680331901583, 26.03314517226533908, -227.7900104434697539 ) ) ;
#10175 = AXIS2_PLACEMENT_3D ( 'NONE', #13372, #5332, #15184 ) ;
#10176 = CARTESIAN_POINT ( 'NONE',  ( 21.60524407607017849, 3.028118258437591415, -217.8361640396714449 ) ) ;
#10177 = CARTESIAN_POINT ( 'NONE',  ( 4.343570314325058135, -14.31236505836544026, -220.3716640818165615 ) ) ;
#10178 = CARTESIAN_POINT ( 'NONE',  ( -18.94992041651601156, 14.87246523864368974, -232.0280096192260828 ) ) ;
#10179 = CARTESIAN_POINT ( 'NONE',  ( -4.866400999161825780, 25.69921167300892861, -231.0100031340613782 ) ) ;
#10180 = EDGE_CURVE ( 'NONE', #3040, #14043, #14854, .T. ) ;
#10181 = CARTESIAN_POINT ( 'NONE',  ( -14.13781561609191328, -15.90667165809925621, -233.6615929499251649 ) ) ;
#10182 = CARTESIAN_POINT ( 'NONE',  ( 15.51129552754472307, 0.2180314803830030457, -231.3815478022924879 ) ) ;
#10183 = CARTESIAN_POINT ( 'NONE',  ( 7.739849882373770917, 11.59357455229016409, -219.5521933286238720 ) ) ;
#10184 = CARTESIAN_POINT ( 'NONE',  ( 15.12287735332712835, 21.03907941686458116, -231.7894952627153202 ) ) ;
#10185 = CARTESIAN_POINT ( 'NONE',  ( 22.30453140437255044, -8.121595866981794032, -232.1448055058014575 ) ) ;
#10186 = CARTESIAN_POINT ( 'NONE',  ( 16.80562970167152415, -4.609754314392994878, -232.4812892975905356 ) ) ;
#10187 = CYLINDRICAL_SURFACE ( 'NONE', #17434, 21.00000000000008171 ) ;
#10188 = CARTESIAN_POINT ( 'NONE',  ( -0.1571923090946999446, 19.34188126963334398, -216.6893131123363787 ) ) ;
#10189 = CARTESIAN_POINT ( 'NONE',  ( -29.73963803141277396, -7.146848409970624871, -220.9878827551818858 ) ) ;
#10190 = CARTESIAN_POINT ( 'NONE',  ( -11.06377138986482933, -15.30386857868810857, -217.0411070525910873 ) ) ;
#10191 = VECTOR ( 'NONE', #14442, 1000.000000000000000 ) ;
#10192 = CARTESIAN_POINT ( 'NONE',  ( 9.584731462935641488, -12.36622837314704348, -230.4796538097028531 ) ) ;
#10193 = CIRCLE ( 'NONE', #17391, 21.80000000000008598 ) ;
#10194 = CARTESIAN_POINT ( 'NONE',  ( -13.30451247859013897, 19.85560227862636040, -232.3493821534129609 ) ) ;
#10195 = CARTESIAN_POINT ( 'NONE',  ( 5.549682179574114471, 15.11687613544382280, -226.9959476502473308 ) ) ;
#10196 = CARTESIAN_POINT ( 'NONE',  ( -13.11494368899652052, 3.355507568391938200, -225.9121440085824304 ) ) ;
#10197 = CARTESIAN_POINT ( 'NONE',  ( -26.47501633019681577, 13.84484755257420119, -230.0154374881822719 ) ) ;
#10198 = CARTESIAN_POINT ( 'NONE',  ( -12.84507615163359873, -10.94093879717347129, -227.8208865714805142 ) ) ;
#10199 = EDGE_LOOP ( 'NONE', ( #2549, #6551, #14923, #2408, #17381, #12582, #817 ) ) ;
#10200 = CARTESIAN_POINT ( 'NONE',  ( -13.51991436508781597, 16.61129329384914755, -232.1184346153593197 ) ) ;
#10201 = CARTESIAN_POINT ( 'NONE',  ( 21.38922145650625239, 17.10616209967719215, -217.8354246241890451 ) ) ;
#10202 = CARTESIAN_POINT ( 'NONE',  ( 21.77779027533950540, 18.43917590911969029, -232.9503911151153659 ) ) ;
#10203 = CARTESIAN_POINT ( 'NONE',  ( 12.85536293311005451, -7.423602990911125410, -229.4216632760384300 ) ) ;
#10204 = DIRECTION ( 'NONE',  ( -1.000000000000000000, 0.000000000000000000, 0.000000000000000000 ) ) ;
#10205 = EDGE_LOOP ( 'NONE', ( #18675, #2588, #9433, #11530 ) ) ;
#10206 = CARTESIAN_POINT ( 'NONE',  ( -1.881996891245037995, 28.05344686410985489, -218.6379207300106202 ) ) ;
#10207 = CARTESIAN_POINT ( 'NONE',  ( -9.208465596459861402, -9.574166310164313742, -220.4340298767933177 ) ) ;
#10208 = CARTESIAN_POINT ( 'NONE',  ( 18.76166303929371537, 3.000000000000002665, -224.9999999999997442 ) ) ;
#10209 = CARTESIAN_POINT ( 'NONE',  ( 15.89706143421296147, 10.57416387607782227, -218.3862415393350318 ) ) ;
#10210 = CARTESIAN_POINT ( 'NONE',  ( -14.87984907657228639, 0.2138881189739126887, -228.7773920408832282 ) ) ;
#10211 = TOROIDAL_SURFACE ( 'NONE', #2640, 24.63401512838747820, 3.000000000000000888 ) ;
#10212 = CARTESIAN_POINT ( 'NONE',  ( 11.43609017326686050, -13.06727081285745307, -217.8903327850316316 ) ) ;
#10213 = CARTESIAN_POINT ( 'NONE',  ( -14.00380962569832199, 8.747390586476997854, -231.7950903513155936 ) ) ;
#10214 = CARTESIAN_POINT ( 'NONE',  ( 16.49791052269847569, 3.745513941566326999, -220.1874559167976884 ) ) ;
#10215 = CARTESIAN_POINT ( 'NONE',  ( -2.609511328024065602, -16.97143768612226822, -230.2205646068415490 ) ) ;
#10216 = DIRECTION ( 'NONE',  ( -1.000000000000000000, 1.224646799147352714E-16, 0.000000000000000000 ) ) ;
#10217 = CARTESIAN_POINT ( 'NONE',  ( 22.18132842682159733, 5.591149267797686839, -232.0584733989884114 ) ) ;
#10218 = CARTESIAN_POINT ( 'NONE',  ( -15.23434562258889891, -0.4010941804143903222, -220.4743703065900036 ) ) ;
#10219 = CARTESIAN_POINT ( 'NONE',  ( 11.49416291172809856, -12.02598964588280595, -221.0946228713814889 ) ) ;
#10221 = EDGE_CURVE ( 'NONE', #8365, #12271, #4961, .T. ) ;
#10220 = CARTESIAN_POINT ( 'NONE',  ( 13.16198298396986743, -2.194854683017246622, -227.0464278254075623 ) ) ;
#10222 = CARTESIAN_POINT ( 'NONE',  ( -20.87479324910686529, -9.656827299161456324, -2.618089337444236442 ) ) ;
#10223 = CARTESIAN_POINT ( 'NONE',  ( 10.12648780932046755, 24.76571117977573522, -228.8499436907259792 ) ) ;
#10224 = CARTESIAN_POINT ( 'NONE',  ( 5.563568780623874943, 21.86458082533069103, -218.6474243140849012 ) ) ;
#10225 = CARTESIAN_POINT ( 'NONE',  ( 8.556785575048143855, -8.471343838569373119, -226.7940772732511050 ) ) ;
#10226 = CARTESIAN_POINT ( 'NONE',  ( 20.38902395782249144, -18.95772103455488633, -230.9098670703349967 ) ) ;
#10227 = ORIENTED_EDGE ( 'NONE', *, *, #1264, .T. ) ;
#10228 = CARTESIAN_POINT ( 'NONE',  ( -10.91003322996498071, 12.84665145358222382, -229.9786893781767958 ) ) ;
#10229 = CARTESIAN_POINT ( 'NONE',  ( -21.26441444091935296, 10.69428164102106926, -219.3434466924981336 ) ) ;
#10230 = CARTESIAN_POINT ( 'NONE',  ( 19.79854089336508594, 4.557290221971136646, -217.3342919181881143 ) ) ;
#10231 = EDGE_LOOP ( 'NONE', ( #19433, #12314, #11695, #9254 ) ) ;
#10232 = CARTESIAN_POINT ( 'NONE',  ( -13.20043892455957746, -23.63849784199488369, -228.2145582502841989 ) ) ;
#10233 = CARTESIAN_POINT ( 'NONE',  ( 15.50884165284638705, 1.028647572718199843, -227.8181348745474679 ) ) ;
#10234 = VERTEX_POINT ( 'NONE', #17345 ) ;
#10235 = ORIENTED_EDGE ( 'NONE', *, *, #13403, .F. ) ;
#10236 = CARTESIAN_POINT ( 'NONE',  ( 13.89183999136464820, 6.553741795688899252, -220.8646181278399752 ) ) ;
#10237 = CARTESIAN_POINT ( 'NONE',  ( 13.77063830053042892, -24.19668776886549821, -225.6207953771408086 ) ) ;
#10238 = EDGE_CURVE ( 'NONE', #3103, #4932, #17133, .T. ) ;
#10239 = CARTESIAN_POINT ( 'NONE',  ( 4.543450689403089271, 15.91052110650461771, -218.9437823786444426 ) ) ;
#10240 = CARTESIAN_POINT ( 'NONE',  ( -15.66530208164916260, 23.23467148471576849, -218.1250122661128046 ) ) ;
#10241 = CARTESIAN_POINT ( 'NONE',  ( 7.359401564398577733, 15.81697286067417707, -215.8326977948377987 ) ) ;
#10242 = CARTESIAN_POINT ( 'NONE',  ( -18.70090456008720992, 23.36146401084868884, -220.3989740370807056 ) ) ;
#10243 = CARTESIAN_POINT ( 'NONE',  ( -2.808235066048971440, 30.42019778760651150, -222.6481917607299295 ) ) ;
#10244 = CIRCLE ( 'NONE', #5182, 25.00000000000000000 ) ;
#10245 = CARTESIAN_POINT ( 'NONE',  ( -25.00000000000013500, 1.224646799147555402E-15, 10.00000000000000000 ) ) ;
#10246 = CARTESIAN_POINT ( 'NONE',  ( 4.201723131641114328, -20.76291977712905279, -215.9522215885928347 ) ) ;
#10247 =( GEOMETRIC_REPRESENTATION_CONTEXT ( 3 ) GLOBAL_UNCERTAINTY_ASSIGNED_CONTEXT ( ( #18429 ) ) GLOBAL_UNIT_ASSIGNED_CONTEXT ( ( #3111, #12945, #11257 ) ) REPRESENTATION_CONTEXT ( 'NONE', 'WORKASPACE' ) );
#10248 = DIRECTION ( 'NONE',  ( 1.000000000000000000, 0.000000000000000000, -0.000000000000000000 ) ) ;
#10249 = DIRECTION ( 'NONE',  ( -1.000000000000000000, 0.000000000000000000, 0.000000000000000000 ) ) ;
#10250 = CARTESIAN_POINT ( 'NONE',  ( -25.95884575339096401, -1.972114683626720044, -231.2145524501483749 ) ) ;
#10251 = CARTESIAN_POINT ( 'NONE',  ( 18.60971343765040942, 2.368090295052050820, -218.6871071987073094 ) ) ;
#10252 = CARTESIAN_POINT ( 'NONE',  ( -16.33212578464095799, -13.18764990320557118, -218.7248530738716283 ) ) ;
#10253 = CARTESIAN_POINT ( 'NONE',  ( 1.366658787427950772, -15.59113167952139456, -228.2894046839634257 ) ) ;
#10254 = CARTESIAN_POINT ( 'NONE',  ( -25.44919589272258520, 4.740781954932180575, -232.0725131810460766 ) ) ;
#10255 = CARTESIAN_POINT ( 'NONE',  ( -2.435715273212520238, 23.41098772907853132, -217.6796576669356966 ) ) ;
#10256 = CARTESIAN_POINT ( 'NONE',  ( -8.894613172508529786, 25.42460746921206294, -232.3150764041658363 ) ) ;
#10257 = ORIENTED_EDGE ( 'NONE', *, *, #18574, .F. ) ;
#10258 = CARTESIAN_POINT ( 'NONE',  ( 23.66932040738428356, 1.377632087272899541, -234.6098499860491415 ) ) ;
#10259 = EDGE_LOOP ( 'NONE', ( #12552, #632 ) ) ;
#10260 = CARTESIAN_POINT ( 'NONE',  ( 20.41153371889344825, 17.18812948447019551, -230.7531656956970778 ) ) ;
#10261 = CARTESIAN_POINT ( 'NONE',  ( -26.47320305716024791, 9.675235842009668019, -228.3542180911597654 ) ) ;
#10262 = CARTESIAN_POINT ( 'NONE',  ( -11.39536650977235510, 9.246300577217761330, -228.4898727004871546 ) ) ;
#10263 = CARTESIAN_POINT ( 'NONE',  ( -14.34029329777712469, -14.57793623142476669, -217.2545494607695389 ) ) ;
#10264 = EDGE_CURVE ( 'NONE', #19076, #13087, #21299, .T. ) ;
#10265 = CIRCLE ( 'NONE', #4132, 1.000000000000000888 ) ;
#10266 = CIRCLE ( 'NONE', #18887, 2.000000000000000000 ) ;
#10267 = FACE_OUTER_BOUND ( 'NONE', #2769, .T. ) ;
#10268 = DIRECTION ( 'NONE',  ( -0.000000000000000000, -0.000000000000000000, 1.000000000000000000 ) ) ;
#10269 = CARTESIAN_POINT ( 'NONE',  ( -21.47149190714903710, 3.672831083387290363, -231.0833634068433469 ) ) ;
#10270 = CARTESIAN_POINT ( 'NONE',  ( 12.48419387172699579, 6.663456953110941328, -219.2717027540951165 ) ) ;
#10271 = CARTESIAN_POINT ( 'NONE',  ( 16.49791052269847569, 3.745513941566326999, -220.1874559167976884 ) ) ;
#10272 = CARTESIAN_POINT ( 'NONE',  ( -15.77287877451090203, -21.23371664991514152, -233.2776952697515185 ) ) ;
#10273 = ORIENTED_EDGE ( 'NONE', *, *, #21568, .F. ) ;
#10274 = CARTESIAN_POINT ( 'NONE',  ( -19.02606456345395358, -20.49905271945607055, -219.9673098173381902 ) ) ;
#10275 = CARTESIAN_POINT ( 'NONE',  ( -10.14083745617744547, 19.87482866967577877, -216.0596634563153486 ) ) ;
#10276 = CARTESIAN_POINT ( 'NONE',  ( 8.115778909262310492, -29.92983049028717346, -224.5060555478150377 ) ) ;
#10277 = CARTESIAN_POINT ( 'NONE',  ( -11.33137429837660193, 27.25022425932026238, -230.1650924901870212 ) ) ;
#10278 = CARTESIAN_POINT ( 'NONE',  ( 13.62633932172415641, -0.5436634383532278347, -227.0682007726617542 ) ) ;
#10279 = CARTESIAN_POINT ( 'NONE',  ( -14.78079095050690661, -5.416970230978240153, -229.7193632018645246 ) ) ;
#10280 = CIRCLE ( 'NONE', #4510, 17.50000000000007816 ) ;
#10281 = CARTESIAN_POINT ( 'NONE',  ( -15.30864812529618391, 1.596444765892653717, -220.3859421844601627 ) ) ;
#10282 = CARTESIAN_POINT ( 'NONE',  ( 0.000000000000000000, 23.00000000000000000, 75.00000000000000000 ) ) ;
#10283 = CARTESIAN_POINT ( 'NONE',  ( -7.366083718505351818, 19.86648438590005838, -231.8662444779758971 ) ) ;
#10284 = CARTESIAN_POINT ( 'NONE',  ( 15.89621445970763070, 6.639162626453350313, -232.5295318698041456 ) ) ;
#10285 = CARTESIAN_POINT ( 'NONE',  ( 16.38151749656409351, 8.902090001712490874, -231.2955017965201989 ) ) ;
#10286 = CARTESIAN_POINT ( 'NONE',  ( 13.60311248493089131, 7.003372205918751092, -219.1738832909067867 ) ) ;
#10287 = CARTESIAN_POINT ( 'NONE',  ( -3.482364789216947809, -21.46714584935086023, -216.0234696677019883 ) ) ;
#10288 = CARTESIAN_POINT ( 'NONE',  ( 9.169328349715531346, 20.85917603618721472, -214.7000934853629133 ) ) ;
#10289 = DIRECTION ( 'NONE',  ( -1.000000000000000000, 0.000000000000000000, 0.000000000000000000 ) ) ;
#10290 = CARTESIAN_POINT ( 'NONE',  ( 8.479858146824877707, -14.20649975585062563, -220.0175458633526091 ) ) ;
#10291 = CARTESIAN_POINT ( 'NONE',  ( -20.97727766418175932, 9.381545086430262970, -232.5968905491617420 ) ) ;
#10292 = VECTOR ( 'NONE', #4280, 1000.000000000000000 ) ;
#10293 = CARTESIAN_POINT ( 'NONE',  ( -1.301562195391901877, 16.19210386685474390, -220.0867867038183192 ) ) ;
#10294 = CARTESIAN_POINT ( 'NONE',  ( -28.30937415889876618, -7.921132361018833556, -222.9755670691803857 ) ) ;
#10295 = CARTESIAN_POINT ( 'NONE',  ( -15.83894155097017631, 1.950284868793920712, -224.5615909987450038 ) ) ;
#10296 = CARTESIAN_POINT ( 'NONE',  ( 16.71272566993619080, 8.989703107375911273, -217.4612081447889125 ) ) ;
#10297 = VERTEX_POINT ( 'NONE', #129 ) ;
#10298 = CARTESIAN_POINT ( 'NONE',  ( 4.656903975822286768, 13.45000048768594780, -227.6722060245555497 ) ) ;
#10299 = CARTESIAN_POINT ( 'NONE',  ( 21.81705645104102587, -16.14081802208856686, -221.4047148572338131 ) ) ;
#10300 = CARTESIAN_POINT ( 'NONE',  ( 11.20610455198612598, -10.15455062626793037, -220.8168162286965526 ) ) ;
#10301 = FILL_AREA_STYLE ('',( #14131 ) ) ;
#10302 = CARTESIAN_POINT ( 'NONE',  ( 12.18657022793382794, 26.76558097653315471, -221.8882195427397335 ) ) ;
#10303 = CARTESIAN_POINT ( 'NONE',  ( -27.27535713358387781, -16.47971293676793181, -227.4585470903502653 ) ) ;
#10304 = CARTESIAN_POINT ( 'NONE',  ( -14.84823930505322132, -23.35465403802561823, -218.3226235040776260 ) ) ;
#10305 = CARTESIAN_POINT ( 'NONE',  ( 8.785770181087007913, -10.38731345016515917, -223.4272116603623317 ) ) ;
#10306 = CARTESIAN_POINT ( 'NONE',  ( -13.71158422780231056, 12.21432067443984693, -232.9166272955793033 ) ) ;
#10307 = CARTESIAN_POINT ( 'NONE',  ( 18.14488609917747652, 6.993670804558928644, -231.4804853770579882 ) ) ;
#10308 = CARTESIAN_POINT ( 'NONE',  ( -12.31207293045244988, 6.732038552366256923, -221.0952066824360713 ) ) ;
#10309 = CARTESIAN_POINT ( 'NONE',  ( -8.115738378024497379, 16.90402287339461296, -219.0833473190803034 ) ) ;
#10310 = CARTESIAN_POINT ( 'NONE',  ( -20.79829908948044448, -4.820361304162784855, -232.2223801333801703 ) ) ;
#10311 = ORIENTED_EDGE ( 'NONE', *, *, #15458, .T. ) ;
#10312 = CARTESIAN_POINT ( 'NONE',  ( -8.611121136347097860, 17.46802294375265419, -231.5575697815534113 ) ) ;
#10313 = ADVANCED_FACE ( 'NONE', ( #5291 ), #20594, .T. ) ;
#10314 = CARTESIAN_POINT ( 'NONE',  ( 27.69955354773053458, 12.81264626165819287, -221.7750850138309602 ) ) ;
#10315 = CARTESIAN_POINT ( 'NONE',  ( 10.22554538262735413, 24.20440706210576209, -215.6176527921760737 ) ) ;
#10316 = CARTESIAN_POINT ( 'NONE',  ( 16.80562970167152415, -4.609754314392994878, -232.4812892975905356 ) ) ;
#10317 = DIRECTION ( 'NONE',  ( -1.000000000000000000, 0.000000000000000000, 0.000000000000000000 ) ) ;
#10318 = ORIENTED_EDGE ( 'NONE', *, *, #18214, .F. ) ;
#10319 = CARTESIAN_POINT ( 'NONE',  ( -3.082945806077231676, 30.69897765966285874, -224.2387254578930822 ) ) ;
#10320 = CARTESIAN_POINT ( 'NONE',  ( -14.65326448616001898, -2.737518208283025167, -217.6605647598149744 ) ) ;
#10321 = FACE_OUTER_BOUND ( 'NONE', #4817, .T. ) ;
#10322 = CARTESIAN_POINT ( 'NONE',  ( 15.87442104186276381, 8.674488492264579520, -230.9702037640878416 ) ) ;
#10323 = CARTESIAN_POINT ( 'NONE',  ( -28.99926036811508467, 3.909990568804979194, -228.9613767892386988 ) ) ;
#10324 = CARTESIAN_POINT ( 'NONE',  ( 15.84759643368428428, -7.142586963752317608, -231.1761396821659673 ) ) ;
#10325 = CARTESIAN_POINT ( 'NONE',  ( -26.74045434827795020, 12.41518252455047744, -220.4617428697642652 ) ) ;
#10326 = PRODUCT ( '360-Degree Detachable Power Base', '360-Degree Detachable Power Base', '', ( #17963 ) ) ;
#10327 = CARTESIAN_POINT ( 'NONE',  ( -27.82842955277035202, 11.70195273568964112, -227.9294339757464911 ) ) ;
#10328 = CARTESIAN_POINT ( 'NONE',  ( 1.167080303844580058, -21.82675117811238152, -232.1335090276773485 ) ) ;
#10329 = DIRECTION ( 'NONE',  ( -0.000000000000000000, -0.000000000000000000, -1.000000000000000000 ) ) ;
#10330 = CARTESIAN_POINT ( 'NONE',  ( -22.17595030361380637, 6.106954805067214664, 7.925275210824247907 ) ) ;
#10331 = DIRECTION ( 'NONE',  ( -0.000000000000000000, -0.000000000000000000, -1.000000000000000000 ) ) ;
#10332 = CARTESIAN_POINT ( 'NONE',  ( 21.15565078817875388, -13.66792796406074295, -219.8984673185389624 ) ) ;
#10333 = CARTESIAN_POINT ( 'NONE',  ( 13.05726252127442244, -2.202320777661724183, -222.9558992616623812 ) ) ;
#10334 = CARTESIAN_POINT ( 'NONE',  ( -20.77537792095403546, -9.868577331483782800, 1.649091285295470444 ) ) ;
#10335 = CARTESIAN_POINT ( 'NONE',  ( 10.48640380280471618, 25.27581435651469022, -227.8976696013017715 ) ) ;
#10336 = CARTESIAN_POINT ( 'NONE',  ( 3.100794261777709782, 20.70580715608724276, -231.8781843337728219 ) ) ;
#10337 = CARTESIAN_POINT ( 'NONE',  ( 5.902215564816073012, -11.20991439657816358, -226.4118943921501170 ) ) ;
#10338 = CARTESIAN_POINT ( 'NONE',  ( 11.90144651507291051, -8.898305237537579515, -228.5592478859710184 ) ) ;
#10339 = ORIENTED_EDGE ( 'NONE', *, *, #17263, .F. ) ;
#10340 = CARTESIAN_POINT ( 'NONE',  ( -11.16203726658389606, 26.27101666727781648, -227.8592829514190612 ) ) ;
#10341 = CARTESIAN_POINT ( 'NONE',  ( -20.41147829968989313, 3.432784889297933795, -230.9611049257633510 ) ) ;
#10342 = CARTESIAN_POINT ( 'NONE',  ( -24.69837543585720141, 12.57569301576483589, -232.4521327773205428 ) ) ;
#10343 = ORIENTED_EDGE ( 'NONE', *, *, #21404, .T. ) ;
#10344 = CARTESIAN_POINT ( 'NONE',  ( -12.44689724543316522, -19.26441470091720731, -219.1960634559673622 ) ) ;
#10345 = DIRECTION ( 'NONE',  ( 1.000000000000000000, -0.000000000000000000, -0.000000000000000000 ) ) ;
#10346 = ORIENTED_EDGE ( 'NONE', *, *, #756, .F. ) ;
#10347 = CARTESIAN_POINT ( 'NONE',  ( 13.59483335902903178, 5.678732573479117640, -228.5032236586631313 ) ) ;
#10348 = CARTESIAN_POINT ( 'NONE',  ( 12.66847874168482591, -12.52481328540277161, -229.3043100997535646 ) ) ;
#10349 = CARTESIAN_POINT ( 'NONE',  ( 15.91295838535984331, 21.88410254487826379, -230.9583961155862823 ) ) ;
#10350 = CARTESIAN_POINT ( 'NONE',  ( -7.429838964355703901, 14.87322129099639234, -232.2632863647814077 ) ) ;
#10351 = EDGE_CURVE ( 'NONE', #20901, #15752, #22187, .T. ) ;
#10352 = CARTESIAN_POINT ( 'NONE',  ( 13.85207896949186335, 7.847214149978243292, -217.3457543576531066 ) ) ;
#10353 = CARTESIAN_POINT ( 'NONE',  ( 0.6364901924797052857, 13.89978473517355617, -221.8840706290426397 ) ) ;
#10354 = DIRECTION ( 'NONE',  ( 0.000000000000000000, 0.000000000000000000, -1.000000000000000000 ) ) ;
#10355 = CARTESIAN_POINT ( 'NONE',  ( 3.342529885312644833, -17.78621320651278737, -216.7788622297345853 ) ) ;
#10356 = CARTESIAN_POINT ( 'NONE',  ( 25.46470895113276711, -14.41152162994631070, -228.1811935238409035 ) ) ;
#10357 = DIRECTION ( 'NONE',  ( 0.000000000000000000, 1.000000000000000000, 0.000000000000000000 ) ) ;
#10358 = CARTESIAN_POINT ( 'NONE',  ( 0.000000000000000000, 0.000000000000000000, 75.00000000000000000 ) ) ;
#10359 = CARTESIAN_POINT ( 'NONE',  ( -25.32262741784088078, 2.623212696197013472, -234.6011982779809841 ) ) ;
#10360 = CARTESIAN_POINT ( 'NONE',  ( -12.55242351043508542, -12.71283815946331686, -230.7436264644880737 ) ) ;
#10361 = CARTESIAN_POINT ( 'NONE',  ( 11.12240951639491549, -23.90857633046665853, -218.9373339142375130 ) ) ;
#10362 = CARTESIAN_POINT ( 'NONE',  ( -24.79507334250576278, 6.844873424762779379, -218.1074956078844878 ) ) ;
#10363 = CARTESIAN_POINT ( 'NONE',  ( 7.772443558932104146, 25.24620711463332157, -231.7813173736589931 ) ) ;
#10364 = CARTESIAN_POINT ( 'NONE',  ( -5.607934827417612844, 15.68271927908880770, -232.1026723719274969 ) ) ;
#10365 = ORIENTED_EDGE ( 'NONE', *, *, #16077, .F. ) ;
#10366 = CARTESIAN_POINT ( 'NONE',  ( 12.49911899277810434, -1.774523103166953497, -229.0731493570444002 ) ) ;
#10367 = ORIENTED_EDGE ( 'NONE', *, *, #15468, .F. ) ;
#10368 = CARTESIAN_POINT ( 'NONE',  ( 22.86997486125673618, 17.56009411325475966, -222.3578648042903296 ) ) ;
#10369 = CARTESIAN_POINT ( 'NONE',  ( -11.39536650977235510, 9.246300577217761330, -228.4898727004871546 ) ) ;
#10370 = CARTESIAN_POINT ( 'NONE',  ( -25.94982248293519689, 10.67899231259548287, -221.1273147719203962 ) ) ;
#10371 = CARTESIAN_POINT ( 'NONE',  ( -8.011291865669539547, -12.94570094964118923, -221.6322823144945744 ) ) ;
#10372 = AXIS2_PLACEMENT_3D ( 'NONE', #16482, #7602, #6232 ) ;
#10373 = FACE_OUTER_BOUND ( 'NONE', #12248, .T. ) ;
#10374 = CARTESIAN_POINT ( 'NONE',  ( 20.05202556141620107, 8.012988804822112954, -215.8722494878839200 ) ) ;
#10375 = CARTESIAN_POINT ( 'NONE',  ( -18.09605518090995702, 22.22778748761825085, -222.5443354630425290 ) ) ;
#10376 = CARTESIAN_POINT ( 'NONE',  ( 14.82579616070250417, 22.96152595385638762, -233.8920860146931489 ) ) ;
#10377 = CARTESIAN_POINT ( 'NONE',  ( 24.78222556642275620, 17.97262539535998371, -226.6641400693514470 ) ) ;
#10378 = CARTESIAN_POINT ( 'NONE',  ( -27.51824122704870135, -10.15715933399136617, -232.3556155038515669 ) ) ;
#10379 = ORIENTED_EDGE ( 'NONE', *, *, #6067, .F. ) ;
#10380 = CARTESIAN_POINT ( 'NONE',  ( -6.776147227169700749, -16.68571135823561846, -231.0772860317820232 ) ) ;
#10381 = ADVANCED_FACE ( 'NONE', ( #6997 ), #20580, .F. ) ;
#10382 = CIRCLE ( 'NONE', #16132, 25.00000000000000000 ) ;
#10383 = CARTESIAN_POINT ( 'NONE',  ( -13.17897211815351000, 23.48099580033777301, -217.3415693533541173 ) ) ;
#10384 = CARTESIAN_POINT ( 'NONE',  ( 8.709470447750865318, -17.43408031369701661, -216.5121658579468829 ) ) ;
#10385 = CARTESIAN_POINT ( 'NONE',  ( 1.382955251742491898, 16.46353944795171032, -231.7743150979565030 ) ) ;
#10386 = CARTESIAN_POINT ( 'NONE',  ( 18.17041142304332624, -16.27896884253082987, -234.9734867155044356 ) ) ;
#10387 = CARTESIAN_POINT ( 'NONE',  ( -14.76273180397945772, -6.370707202906876532, -220.0066229284273334 ) ) ;
#10388 = ADVANCED_FACE ( 'NONE', ( #10267 ), #19876, .T. ) ;
#10389 = CARTESIAN_POINT ( 'NONE',  ( -21.43408368508570305, 3.680162304907783621, -233.1134812316964542 ) ) ;
#10390 = DIRECTION ( 'NONE',  ( 0.000000000000000000, 0.000000000000000000, -1.000000000000000000 ) ) ;
#10391 = CARTESIAN_POINT ( 'NONE',  ( -2.015708574708954259, 26.78900769828807782, -221.5371848586876808 ) ) ;
#10392 = CARTESIAN_POINT ( 'NONE',  ( -25.44919589272258520, 4.740781954932180575, -232.0725131810460766 ) ) ;
#10393 = CARTESIAN_POINT ( 'NONE',  ( 13.43170911749896490, 19.07691563292472026, -232.7497845103644636 ) ) ;
#10394 = CARTESIAN_POINT ( 'NONE',  ( 22.22999428328319382, 14.15012104770485557, -232.1858878619060249 ) ) ;
#10395 = CARTESIAN_POINT ( 'NONE',  ( 5.521532699605532279, -19.36944961733043513, -235.0341191922501594 ) ) ;
#10396 = CARTESIAN_POINT ( 'NONE',  ( 2.631948090663005946, 31.21493676147814611, -222.3107766067421380 ) ) ;
#10397 = CARTESIAN_POINT ( 'NONE',  ( 0.000000000000000000, 0.000000000000000000, -30.00000000000000000 ) ) ;
#10398 = CARTESIAN_POINT ( 'NONE',  ( 1.345830553852720657, -29.56269728401072783, -219.9360760428637604 ) ) ;
#10399 = CARTESIAN_POINT ( 'NONE',  ( -17.08384421609436643, 23.56421365837046622, -225.2902702884460666 ) ) ;
#10400 = CARTESIAN_POINT ( 'NONE',  ( -1.975202609796049336, 20.81351768191813889, -217.5779402428482001 ) ) ;
#10401 = CARTESIAN_POINT ( 'NONE',  ( -21.80830016239255897, -4.781675611938959847, -217.4666014280278148 ) ) ;
#10402 = CARTESIAN_POINT ( 'NONE',  ( -24.40185606299549192, 11.66496215664722236, -221.9473669705449765 ) ) ;
#10403 = CARTESIAN_POINT ( 'NONE',  ( -10.95054816480499760, 8.339404316518379545, -224.1596700080921778 ) ) ;
#10404 = CARTESIAN_POINT ( 'NONE',  ( 19.66122710937851537, 22.83208755991274330, -220.0578523118790883 ) ) ;
#10405 = CARTESIAN_POINT ( 'NONE',  ( 10.50530447320976535, 20.19629329636330084, -217.1354359361034767 ) ) ;
#10406 = CARTESIAN_POINT ( 'NONE',  ( 14.36131679319511001, -8.144601358551431858, -221.7207256223857144 ) ) ;
#10407 = EDGE_LOOP ( 'NONE', ( #4657, #6829 ) ) ;
#10408 = CARTESIAN_POINT ( 'NONE',  ( 24.96165930385824794, -17.14663603160204275, -224.2745859498249672 ) ) ;
#10409 = CARTESIAN_POINT ( 'NONE',  ( -2.693916085894628942, 18.86613858709357672, -230.4911878356387263 ) ) ;
#10410 = CARTESIAN_POINT ( 'NONE',  ( 22.56777165119825668, 0.000000000000000000, 93.00000000000000000 ) ) ;
#10411 = CARTESIAN_POINT ( 'NONE',  ( 14.32085100525799248, 9.220655089380342062, -219.9006227404039464 ) ) ;
#10412 = CARTESIAN_POINT ( 'NONE',  ( -18.70843642779997040, -17.48186590846855992, -215.2841814587906981 ) ) ;
#10413 = CARTESIAN_POINT ( 'NONE',  ( -1.633632075387274840, -15.48245080501611071, -218.5193615163172751 ) ) ;
#10414 = CARTESIAN_POINT ( 'NONE',  ( 15.11994912051959972, -12.48385213956034079, -232.8079920308188377 ) ) ;
#10415 = CARTESIAN_POINT ( 'NONE',  ( -3.504118661534079582, 16.69899759879061918, -221.4378787282527128 ) ) ;
#10416 = CYLINDRICAL_SURFACE ( 'NONE', #11251, 21.50000000000001066 ) ;
#10417 = CARTESIAN_POINT ( 'NONE',  ( 14.72648027392381387, 10.15511732729369676, -229.5776536674053716 ) ) ;
#10418 = CARTESIAN_POINT ( 'NONE',  ( -14.00380962569832199, 8.747390586476997854, -231.7950903513155936 ) ) ;
#10419 = CARTESIAN_POINT ( 'NONE',  ( -15.63515374589483109, 24.59141623553136569, -226.9057426066772507 ) ) ;
#10420 = CARTESIAN_POINT ( 'NONE',  ( 30.81364357021286793, -2.580535071768633060, -224.0234450364292513 ) ) ;
#10421 = CARTESIAN_POINT ( 'NONE',  ( 1.939863782649466017, 28.20584428268631783, -229.4487744520996273 ) ) ;
#10422 = CARTESIAN_POINT ( 'NONE',  ( -20.41147829968989313, 3.432784889297933795, -230.9611049257633510 ) ) ;
#10423 = CARTESIAN_POINT ( 'NONE',  ( 11.13671218404335761, 30.21738803452449673, -224.2405745632392211 ) ) ;
#10424 = CARTESIAN_POINT ( 'NONE',  ( 4.823266655078461085, -13.86048651889774241, -224.7145696108100026 ) ) ;
#10425 = LINE ( 'NONE', #8741, #4602 ) ;
#10426 = ORIENTED_EDGE ( 'NONE', *, *, #14102, .T. ) ;
#10427 = CARTESIAN_POINT ( 'NONE',  ( -6.474151797443945533, 21.29193859232740138, -215.9573456447696458 ) ) ;
#10428 = CARTESIAN_POINT ( 'NONE',  ( -10.76816654174163368, -5.786055782404167402, -221.6662823521482437 ) ) ;
#10429 = ADVANCED_FACE ( 'NONE', ( #10373 ), #9469, .T. ) ;
#10430 = CARTESIAN_POINT ( 'NONE',  ( 0.000000000000000000, 19.79999999999999716, 78.50000000000000000 ) ) ;
#10431 = CARTESIAN_POINT ( 'NONE',  ( 26.29894631880581812, 12.29609390142961090, -226.3100047295820332 ) ) ;
#10432 = CARTESIAN_POINT ( 'NONE',  ( -29.88125065636863198, 4.504452993877526623, -226.2048141718237275 ) ) ;
#10433 = CARTESIAN_POINT ( 'NONE',  ( 18.00123703865980218, -15.82960056198189491, -233.0014896689109776 ) ) ;
#10434 = SHAPE_REPRESENTATION_RELATIONSHIP ( 'NONE' , 'NONE' ,  #13052, #11503 ) ;
#10435 = CARTESIAN_POINT ( 'NONE',  ( -11.02345917017863464, 29.02019856777526741, -223.9475008740665771 ) ) ;
#10436 = CARTESIAN_POINT ( 'NONE',  ( -28.13472254077564116, 12.33996625515159629, -224.9141344439281909 ) ) ;
#10437 = CARTESIAN_POINT ( 'NONE',  ( -1.615718423935818437, -15.01490656935555812, -223.2481059054151729 ) ) ;
#10438 = CARTESIAN_POINT ( 'NONE',  ( 1.232595164407830946E-29, -17.50000000000007105, -55.00000000000000000 ) ) ;
#10439 = CARTESIAN_POINT ( 'NONE',  ( 16.91879448796214191, 0.8271603773820436212, -230.0510230802265710 ) ) ;
#10440 = CARTESIAN_POINT ( 'NONE',  ( -16.63766460830045091, 5.158675778507696208, -232.1659425527909093 ) ) ;
#10441 = CARTESIAN_POINT ( 'NONE',  ( 17.09791731880535437, -14.50769433911838568, -231.1780219065761059 ) ) ;
#10442 = CARTESIAN_POINT ( 'NONE',  ( 13.78122601621266519, -1.862995838536092519, -227.3514709470891546 ) ) ;
#10443 = CARTESIAN_POINT ( 'NONE',  ( -22.97017636999641255, 9.867926576900321933, 1.652878766021345758 ) ) ;
#10444 = CARTESIAN_POINT ( 'NONE',  ( 15.70179827786738969, 6.572001003133339125, -229.5476218741844434 ) ) ;
#10445 = CARTESIAN_POINT ( 'NONE',  ( -12.19796877179171446, 17.24929682309303658, -234.5722138766719809 ) ) ;
#10446 = CARTESIAN_POINT ( 'NONE',  ( 14.37653162493774239, 9.985418694807894013, -229.1686718965858063 ) ) ;
#10447 = CARTESIAN_POINT ( 'NONE',  ( 3.722478027540565559, -17.18860102498078390, -232.3439289206262686 ) ) ;
#10448 = CARTESIAN_POINT ( 'NONE',  ( 14.15946391865398013, -0.7413617426029489588, -228.5799580636366670 ) ) ;
#10449 = ORIENTED_EDGE ( 'NONE', *, *, #21201, .F. ) ;
#10450 = CARTESIAN_POINT ( 'NONE',  ( 1.939863782649466017, 28.20584428268631783, -229.4487744520996273 ) ) ;
#10451 = CARTESIAN_POINT ( 'NONE',  ( -15.32935061426341861, 5.146212415319166844, -225.5669090095357774 ) ) ;
#10452 = CARTESIAN_POINT ( 'NONE',  ( -22.28357709049062407, 7.264818440526320309, -215.3877468064711707 ) ) ;
#10453 = CARTESIAN_POINT ( 'NONE',  ( -3.373690338999510985, -20.30281967708846125, -218.2431319494177160 ) ) ;
#10454 = CARTESIAN_POINT ( 'NONE',  ( 0.000000000000000000, 0.000000000000000000, 77.51594804401857175 ) ) ;
#10455 = ORIENTED_EDGE ( 'NONE', *, *, #4443, .T. ) ;
#10456 = CARTESIAN_POINT ( 'NONE',  ( 16.71272566993619080, 8.989703107375911273, -217.4612081447889125 ) ) ;
#10457 = CARTESIAN_POINT ( 'NONE',  ( 17.63166870185818169, -20.21345786093278107, -221.6360081359454739 ) ) ;
#10458 = CARTESIAN_POINT ( 'NONE',  ( 4.484811161826725900, 15.38298568785217313, -219.4617573400562662 ) ) ;
#10459 = CARTESIAN_POINT ( 'NONE',  ( -20.18153419852512442, 14.25141268122526483, -233.5059133483111964 ) ) ;
#10460 = CARTESIAN_POINT ( 'NONE',  ( 19.48863273024974418, 12.80680990455712909, -215.0408095016468053 ) ) ;
#10461 = CARTESIAN_POINT ( 'NONE',  ( 8.812073984913094904, 13.12649198322903210, -229.9172071780580495 ) ) ;
#10462 = CARTESIAN_POINT ( 'NONE',  ( -10.76782065184847781, 0.1824719560092695203, 91.99999999999998579 ) ) ;
#10463 = CARTESIAN_POINT ( 'NONE',  ( -1.632242579688942596, -13.62074943359385415, -221.1585305289511041 ) ) ;
#10464 = CARTESIAN_POINT ( 'NONE',  ( 21.53087031351596892, -21.03550532031109555, -227.1077645633325233 ) ) ;
#10465 = DIRECTION ( 'NONE',  ( 0.000000000000000000, 0.000000000000000000, -1.000000000000000000 ) ) ;
#10466 = DIRECTION ( 'NONE',  ( 1.000000000000000000, 0.000000000000000000, 0.000000000000000000 ) ) ;
#10467 = CARTESIAN_POINT ( 'NONE',  ( -18.07648963816576781, 14.36622924931724654, -235.1425738388569187 ) ) ;
#10468 = CARTESIAN_POINT ( 'NONE',  ( -27.92538795710911259, -2.661554249663629079, -224.6264721727631581 ) ) ;
#10469 = CARTESIAN_POINT ( 'NONE',  ( -29.22672729369577738, 6.588740615114764054, -224.9915299386302934 ) ) ;
#10470 = CARTESIAN_POINT ( 'NONE',  ( -1.038524475621362075, 14.89017051181998141, -222.3948816610352139 ) ) ;
#10471 = CARTESIAN_POINT ( 'NONE',  ( 3.755480357635514022, 24.23367984900377436, -231.4105847235276201 ) ) ;
#10472 = ORIENTED_EDGE ( 'NONE', *, *, #6345, .T. ) ;
#10473 = CARTESIAN_POINT ( 'NONE',  ( 30.80938026993025503, 0.02210899415489638725, -229.5596456628577187 ) ) ;
#10474 = CARTESIAN_POINT ( 'NONE',  ( 7.168644370073567806, 19.32044210858112265, -233.1278450877711634 ) ) ;
#10475 = CARTESIAN_POINT ( 'NONE',  ( -21.66801938871533650, 16.28801167444048659, -218.5240035253498547 ) ) ;
#10476 = CARTESIAN_POINT ( 'NONE',  ( -26.47320305716024791, 9.675235842009668019, -228.3542180911597654 ) ) ;
#10477 = CARTESIAN_POINT ( 'NONE',  ( -18.38002254392888446, -21.81807606669838506, -229.0374583293157968 ) ) ;
#10478 = DIRECTION ( 'NONE',  ( 1.000000000000000000, 0.000000000000000000, 0.000000000000000000 ) ) ;
#10479 = CARTESIAN_POINT ( 'NONE',  ( -24.63401512838761320, 3.016796777712736283E-15, 77.51594804401857175 ) ) ;
#10480 = CARTESIAN_POINT ( 'NONE',  ( 2.999999999999971578, 3.673940397442062826E-16, -221.9999999999999716 ) ) ;
#10481 = CARTESIAN_POINT ( 'NONE',  ( 28.03290210476798094, 13.48017620089690638, -224.9212082181537937 ) ) ;
#10482 = CARTESIAN_POINT ( 'NONE',  ( -13.23768812067001477, 12.78288831771969569, -230.4179793829127902 ) ) ;
#10483 = CARTESIAN_POINT ( 'NONE',  ( 13.32754126089433377, 12.31312334927721963, -234.6033665822900218 ) ) ;
#10484 = CARTESIAN_POINT ( 'NONE',  ( -16.71711190488355570, 0.6105529133557690002, -230.9511258789794681 ) ) ;
#10485 = CARTESIAN_POINT ( 'NONE',  ( -10.57293828068126373, -5.503282544971903611, -227.1466070594375708 ) ) ;
#10486 = AXIS2_PLACEMENT_3D ( 'NONE', #9873, #17075, #16739 ) ;
#10487 = ORIENTED_EDGE ( 'NONE', *, *, #20644, .T. ) ;
#10488 = CARTESIAN_POINT ( 'NONE',  ( -12.96708845633950347, -3.368725568741437026, -223.5528514750533873 ) ) ;
#10489 = CARTESIAN_POINT ( 'NONE',  ( -5.383332542724544645, 15.12651309054520432, -231.5699995578976313 ) ) ;
#10490 = CARTESIAN_POINT ( 'NONE',  ( -11.28700884291539630, -21.85791790461604478, -233.5354093188319951 ) ) ;
#10491 = CARTESIAN_POINT ( 'NONE',  ( -6.201839134465864767, 11.37481922992157379, -223.7040893475979146 ) ) ;
#10492 = CARTESIAN_POINT ( 'NONE',  ( 14.85580775603058079, -28.43502054068834894, -222.5810199743787905 ) ) ;
#10493 = FACE_OUTER_BOUND ( 'NONE', #15989, .T. ) ;
#10494 = ADVANCED_FACE ( 'NONE', ( #11728 ), #3159, .T. ) ;
#10495 = CARTESIAN_POINT ( 'NONE',  ( -18.88895772509644644, 1.306698388790553444, -217.6272550812279292 ) ) ;
#10496 = CARTESIAN_POINT ( 'NONE',  ( -5.706122936196527107, 15.14201253431006045, -228.6865785740211550 ) ) ;
#10497 = CARTESIAN_POINT ( 'NONE',  ( 12.89118769162836031, 6.140251663080722899, -228.8792332048833771 ) ) ;
#10498 = VECTOR ( 'NONE', #13980, 1000.000000000000000 ) ;
#10499 = CARTESIAN_POINT ( 'NONE',  ( 20.89184612657454920, 5.404957034965973683, -232.0952743654565609 ) ) ;
#10500 = CARTESIAN_POINT ( 'NONE',  ( 13.06430160593375689, 2.561628050526134182, -220.6026188403641299 ) ) ;
#10501 = CARTESIAN_POINT ( 'NONE',  ( -4.538939863750555581, -15.27574540357637112, -231.4384328720293524 ) ) ;
#10502 = CARTESIAN_POINT ( 'NONE',  ( 2.000982021813747291, 12.72833461843010205, -228.3416607300594308 ) ) ;
#10503 = DIRECTION ( 'NONE',  ( 0.000000000000000000, 0.000000000000000000, 1.000000000000000000 ) ) ;
#10504 = CARTESIAN_POINT ( 'NONE',  ( -4.110806133445755961, -12.94090688063470473, -230.1197724001632992 ) ) ;
#10505 = CARTESIAN_POINT ( 'NONE',  ( -7.284474494690100776, 13.60812129561547046, -227.7414351104868331 ) ) ;
#10506 = EDGE_CURVE ( 'NONE', #20995, #351, #18812, .T. ) ;
#10507 = CARTESIAN_POINT ( 'NONE',  ( 21.26803326031697949, 19.54255073453192892, -230.5813148908474659 ) ) ;
#10508 = CIRCLE ( 'NONE', #2594, 3.000000000000006217 ) ;
#10509 = CARTESIAN_POINT ( 'NONE',  ( -16.20471097821853235, -2.781505378741172319, -220.1484675126197317 ) ) ;
#10510 = CARTESIAN_POINT ( 'NONE',  ( -17.00819119081011266, 8.904695857470725784, -219.7915043529501133 ) ) ;
#10511 = CARTESIAN_POINT ( 'NONE',  ( -11.40916210110096962, 20.01996232974788725, -234.3205435716851923 ) ) ;
#10512 = CARTESIAN_POINT ( 'NONE',  ( 16.40130693394614525, -0.1574073183566240264, -221.9481963320051534 ) ) ;
#10513 = ORIENTED_EDGE ( 'NONE', *, *, #20477, .F. ) ;
#10514 = CARTESIAN_POINT ( 'NONE',  ( 8.587407344280324040, -17.24386586482343375, -219.6634241328915209 ) ) ;
#10515 = ORIENTED_EDGE ( 'NONE', *, *, #2798, .T. ) ;
#10516 = CARTESIAN_POINT ( 'NONE',  ( 5.037691872308702301, -15.96383311541683270, -230.0422288358542460 ) ) ;
#10517 = CARTESIAN_POINT ( 'NONE',  ( -3.015877970456246615, 27.27456613555083464, -227.6995284396757313 ) ) ;
#10518 = CARTESIAN_POINT ( 'NONE',  ( 7.995304978256253747, 13.28024228361502779, -220.6535174700288451 ) ) ;
#10519 = CARTESIAN_POINT ( 'NONE',  ( 15.13105790938820228, -1.902449014147146178, -222.1588331224812407 ) ) ;
#10520 = CARTESIAN_POINT ( 'NONE',  ( -5.178973235464019886, -24.35492185057628944, -233.6431870320687381 ) ) ;
#10521 = CARTESIAN_POINT ( 'NONE',  ( -0.8413160509385254615, -28.71376977722865931, -218.8117683208458288 ) ) ;
#10522 = CARTESIAN_POINT ( 'NONE',  ( -8.752190949579933488, 24.25633523490762755, -230.6624101830059885 ) ) ;
#10523 = CYLINDRICAL_SURFACE ( 'NONE', #14143, 3.000000000000002665 ) ;
#10524 = CARTESIAN_POINT ( 'NONE',  ( 15.88536911906737181, 12.85343532334862893, -218.9532478288372204 ) ) ;
#10525 = CARTESIAN_POINT ( 'NONE',  ( -28.13472254077564116, 12.33996625515159629, -224.9141344439281909 ) ) ;
#10526 = CARTESIAN_POINT ( 'NONE',  ( -13.44241955326339166, 15.88952131657459965, -217.2587743382015901 ) ) ;
#10527 = AXIS2_PLACEMENT_3D ( 'NONE', #7022, #13894, #20731 ) ;
#10528 = VERTEX_POINT ( 'NONE', #8583 ) ;
#10529 = TOROIDAL_SURFACE ( 'NONE', #12704, 10.76794919243112325, 2.000000000000000000 ) ;
#10530 = CARTESIAN_POINT ( 'NONE',  ( 3.192353461299334061, 22.13718518159985393, -217.1103300728619843 ) ) ;
#10531 = CARTESIAN_POINT ( 'NONE',  ( -21.48978835671764287, 1.062155088816892468, -219.0000000007146355 ) ) ;
#10532 = CARTESIAN_POINT ( 'NONE',  ( 8.546572992885776543, 19.06776382077057974, -214.7173484156796519 ) ) ;
#10533 = CARTESIAN_POINT ( 'NONE',  ( 12.78854151797817451, -25.92021405714643123, -222.0152117995072842 ) ) ;
#10534 = LINE ( 'NONE', #6117, #13242 ) ;
#10535 = ORIENTED_EDGE ( 'NONE', *, *, #19326, .T. ) ;
#10536 = CARTESIAN_POINT ( 'NONE',  ( 0.2389779871941385414, 16.64595486589868045, -218.1658233406367629 ) ) ;
#10537 = CARTESIAN_POINT ( 'NONE',  ( 17.75464445068659458, -4.950329359371821170, -229.7529072665692240 ) ) ;
#10538 = CARTESIAN_POINT ( 'NONE',  ( 29.12543877365354916, -1.475122899492763873, -224.0746120762670444 ) ) ;
#10539 = CARTESIAN_POINT ( 'NONE',  ( 17.34727976380017722, 4.822939981779328811, -230.8836217450937909 ) ) ;
#10540 = CARTESIAN_POINT ( 'NONE',  ( -14.70651859537745487, 4.211702956367679107, -230.0357207626005334 ) ) ;
#10541 = CARTESIAN_POINT ( 'NONE',  ( 5.609436632608550966, -13.11664087352601094, -229.3324225951633650 ) ) ;
#10542 = DIRECTION ( 'NONE',  ( 0.000000000000000000, 0.000000000000000000, 1.000000000000000000 ) ) ;
#10543 = CARTESIAN_POINT ( 'NONE',  ( -7.395406416482832590, 12.93623984139929739, -219.2606224730616873 ) ) ;
#10544 = AXIS2_PLACEMENT_3D ( 'NONE', #5397, #9438, #13981 ) ;
#10545 = VERTEX_POINT ( 'NONE', #15446 ) ;
#10546 = CARTESIAN_POINT ( 'NONE',  ( -17.84981083811007707, 0.8485253248287054628, -231.8041300026935119 ) ) ;
#10547 = CARTESIAN_POINT ( 'NONE',  ( -8.326748185965973548, -13.59788789161040512, -220.4531618457016862 ) ) ;
#10548 = VECTOR ( 'NONE', #3222, 1000.000000000000000 ) ;
#10549 = DIRECTION ( 'NONE',  ( -1.000000000000000000, 0.000000000000000000, 0.000000000000000000 ) ) ;
#10550 = CARTESIAN_POINT ( 'NONE',  ( -22.03215468537991839, 6.606953063173292229, 7.513524830561480350 ) ) ;
#10551 = CARTESIAN_POINT ( 'NONE',  ( -24.24202834850560606, 19.05981756344202438, -226.6980666352953335 ) ) ;
#10552 = CARTESIAN_POINT ( 'NONE',  ( 23.68557655437113141, -13.81416892717991551, -227.4080549258873987 ) ) ;
#10553 = DIRECTION ( 'NONE',  ( 0.000000000000000000, 0.000000000000000000, 1.000000000000000000 ) ) ;
#10554 = CARTESIAN_POINT ( 'NONE',  ( 14.23294950300690331, 6.961167337017927892, -222.0879133937260974 ) ) ;
#10555 = CARTESIAN_POINT ( 'NONE',  ( -16.89013823391154290, 26.38860451648245231, -225.6449744083545852 ) ) ;
#10556 = DIRECTION ( 'NONE',  ( -1.000000000000000000, 0.000000000000000000, 0.000000000000000000 ) ) ;
#10557 = CARTESIAN_POINT ( 'NONE',  ( 12.84032013659066251, 19.10303921738740485, -230.8110334357214128 ) ) ;
#10558 = CARTESIAN_POINT ( 'NONE',  ( -7.536234698756538286, -25.83616497442384130, -229.4709156672317363 ) ) ;
#10559 = CARTESIAN_POINT ( 'NONE',  ( 28.89510310306777541, -0.2847990887752292477, -220.1812426115722303 ) ) ;
#10560 = VERTEX_POINT ( 'NONE', #17236 ) ;
#10561 = CARTESIAN_POINT ( 'NONE',  ( 1.104227501629593045, 25.05528885094460989, -231.9808705443460326 ) ) ;
#10562 = CARTESIAN_POINT ( 'NONE',  ( -22.36207348798144778, 17.12313795477538036, -223.8571857210765472 ) ) ;
#10563 = CARTESIAN_POINT ( 'NONE',  ( -26.41026844077819291, 5.012316129610852933, -233.8406020309487872 ) ) ;
#10564 = CARTESIAN_POINT ( 'NONE',  ( -23.21124258271143503, -15.80671483884278317, -224.0808897361354468 ) ) ;
#10565 = DIRECTION ( 'NONE',  ( 0.000000000000000000, 0.000000000000000000, 1.000000000000000000 ) ) ;
#10566 = VERTEX_POINT ( 'NONE', #16904 ) ;
#10567 = TOROIDAL_SURFACE ( 'NONE', #849, 13.12488928717151637, 3.000000000000000000 ) ;
#10568 = CARTESIAN_POINT ( 'NONE',  ( 18.55287065739596031, 7.869864349944380777, -232.8430408253643691 ) ) ;
#10569 = CARTESIAN_POINT ( 'NONE',  ( 3.499756879752360827, -15.16424639601953039, -225.9472731234413061 ) ) ;
#10570 = CARTESIAN_POINT ( 'NONE',  ( 20.41153371889344825, 17.18812948447019551, -230.7531656956970778 ) ) ;
#10571 = EDGE_CURVE ( 'NONE', #15054, #11155, #20224, .T. ) ;
#10572 = CARTESIAN_POINT ( 'NONE',  ( -14.00380962569832199, 8.747390586476997854, -231.7950903513155936 ) ) ;
#10573 = CARTESIAN_POINT ( 'NONE',  ( 29.64577750251057608, 2.839131411071813549, -220.9704389295326905 ) ) ;
#10574 = CARTESIAN_POINT ( 'NONE',  ( 7.743212835174657194, 11.90778931056080481, -226.0491028376908105 ) ) ;
#10575 = DIRECTION ( 'NONE',  ( -1.000000000000000000, 0.000000000000000000, 0.000000000000000000 ) ) ;
#10576 = CARTESIAN_POINT ( 'NONE',  ( 1.541778504653760429, -23.48174737203985529, -233.9922866444541967 ) ) ;
#10577 = CARTESIAN_POINT ( 'NONE',  ( 15.05686526350529775, -5.555778903407086133, -220.1433349335996468 ) ) ;
#10578 = CARTESIAN_POINT ( 'NONE',  ( 0.000000000000000000, 19.63401512838754215, 77.51594804401857175 ) ) ;
#10579 = CIRCLE ( 'NONE', #4460, 17.50000000000000711 ) ;
#10580 = DIRECTION ( 'NONE',  ( 0.000000000000000000, 0.000000000000000000, -1.000000000000000000 ) ) ;
#10581 = CARTESIAN_POINT ( 'NONE',  ( -7.694246740028670928, 10.31295298368923063, -221.9989544301487001 ) ) ;
#10582 = CARTESIAN_POINT ( 'NONE',  ( -26.34963598119476913, -8.267085687785165504, -223.3493716711078889 ) ) ;
#10583 = CARTESIAN_POINT ( 'NONE',  ( -18.04772061096520375, 5.916925414182395038, -217.8829197293425750 ) ) ;
#10584 = CARTESIAN_POINT ( 'NONE',  ( 2.951582164238582440, 19.39026647431845873, -217.4356918981242472 ) ) ;
#10585 = CARTESIAN_POINT ( 'NONE',  ( -2.665457046508036942, 16.94988614842223029, -218.7621057649994896 ) ) ;
#10586 = VERTEX_POINT ( 'NONE', #8684 ) ;
#10587 = CARTESIAN_POINT ( 'NONE',  ( 8.556785575048143855, -8.471343838569373119, -226.7940772732511050 ) ) ;
#10588 = VERTEX_POINT ( 'NONE', #12171 ) ;
#10589 = CARTESIAN_POINT ( 'NONE',  ( 25.18785298611088308, 3.974282393449815931, -218.7636041058819956 ) ) ;
#10590 = CARTESIAN_POINT ( 'NONE',  ( -9.251743101293765648, 14.06372330290396278, -232.4239003576353468 ) ) ;
#10591 = EDGE_CURVE ( 'NONE', #13407, #6170, #352, .T. ) ;
#10592 = CARTESIAN_POINT ( 'NONE',  ( -25.19195624009214640, 10.50676406307063182, -220.0954552869889937 ) ) ;
#10593 = CARTESIAN_POINT ( 'NONE',  ( -11.96638064467250473, -24.81952708901905069, -229.8544473269683692 ) ) ;
#10594 = CARTESIAN_POINT ( 'NONE',  ( -13.58874046263339608, 12.73011668665171392, -216.5659449791897941 ) ) ;
#10595 = DIRECTION ( 'NONE',  ( 6.982962677686272233E-15, -1.000000000000000000, 0.000000000000000000 ) ) ;
#10596 = CARTESIAN_POINT ( 'NONE',  ( 20.10109416526603709, 2.018147939476731434, -216.1034161917718848 ) ) ;
#10597 = VECTOR ( 'NONE', #3972, 1000.000000000000000 ) ;
#10598 = CARTESIAN_POINT ( 'NONE',  ( -18.36252859017411510, 21.06344830687906367, -228.5073589488702623 ) ) ;
#10599 =( GEOMETRIC_REPRESENTATION_CONTEXT ( 3 ) GLOBAL_UNCERTAINTY_ASSIGNED_CONTEXT ( ( #1094 ) ) GLOBAL_UNIT_ASSIGNED_CONTEXT ( ( #8420, #22137, #12011 ) ) REPRESENTATION_CONTEXT ( 'NONE', 'WORKASPACE' ) );
#10600 = CARTESIAN_POINT ( 'NONE',  ( 16.84354851290083133, 10.42424693870724361, -215.2582953371023109 ) ) ;
#10601 = CARTESIAN_POINT ( 'NONE',  ( -18.08305592660031991, 4.022743421239192152, -217.2335041149100050 ) ) ;
#10602 = CARTESIAN_POINT ( 'NONE',  ( -27.90711606799872513, 0.4679914357742857023, -216.8754026763949128 ) ) ;
#10603 = CARTESIAN_POINT ( 'NONE',  ( -26.76734473129764069, -3.453818734898710829, -232.3222361544058003 ) ) ;
#10604 = CARTESIAN_POINT ( 'NONE',  ( -4.450022810944913587, 12.45400981846350597, -225.2098051417536340 ) ) ;
#10605 = CARTESIAN_POINT ( 'NONE',  ( -11.40116373163465369, -15.95513543764466213, -216.7841692646331353 ) ) ;
#10606 = CARTESIAN_POINT ( 'NONE',  ( 4.907833106823921376, 13.98151846258800290, -229.0190609869640923 ) ) ;
#10607 = CARTESIAN_POINT ( 'NONE',  ( 19.49551695935633688, -21.73806820219217428, -217.5227155576580742 ) ) ;
#10608 = DIRECTION ( 'NONE',  ( 0.000000000000000000, 0.000000000000000000, 1.000000000000000000 ) ) ;
#10609 = CARTESIAN_POINT ( 'NONE',  ( 20.47387447818710271, 7.390772095927000684, -234.0991886097562258 ) ) ;
#10610 = DIRECTION ( 'NONE',  ( -1.000000000000000000, 0.000000000000000000, -0.000000000000000000 ) ) ;
#10611 = CARTESIAN_POINT ( 'NONE',  ( -3.010752168931037698, 15.84372070116375575, -223.4060793985500482 ) ) ;
#10612 = CARTESIAN_POINT ( 'NONE',  ( 28.53243699394185384, 6.329221954355706004, -218.6437889135959267 ) ) ;
#10613 = CARTESIAN_POINT ( 'NONE',  ( 14.19800769603076240, 4.587407146151301518, -224.2928935459285071 ) ) ;
#10614 = CARTESIAN_POINT ( 'NONE',  ( 18.30177952310522471, 1.918278963380847468, -233.8574151782075887 ) ) ;
#10615 = CARTESIAN_POINT ( 'NONE',  ( -7.242471263717580321, -12.67345288765796774, -222.7008556220510229 ) ) ;
#10616 = CIRCLE ( 'NONE', #4850, 19.63401512838747820 ) ;
#10617 = MECHANICAL_DESIGN_GEOMETRIC_PRESENTATION_REPRESENTATION (  '', ( #7747 ), #4134 ) ;
#10618 = CARTESIAN_POINT ( 'NONE',  ( 15.89102655998366664, 24.10108298038447572, -232.7733025413564008 ) ) ;
#10619 = CARTESIAN_POINT ( 'NONE',  ( 0.000000000000000000, 0.000000000000000000, 75.00000000000000000 ) ) ;
#10620 = CARTESIAN_POINT ( 'NONE',  ( -6.773088999562194346, -28.54379939428971369, -218.3283227997898450 ) ) ;
#10621 = CARTESIAN_POINT ( 'NONE',  ( -16.57767831947938575, 23.50485984366324388, -222.7977068309636763 ) ) ;
#10622 = CARTESIAN_POINT ( 'NONE',  ( 12.96449997971774870, 8.285709878278680662, -230.9518598506670628 ) ) ;
#10623 = ADVANCED_FACE ( 'NONE', ( #21563 ), #14622, .F. ) ;
#10624 = CARTESIAN_POINT ( 'NONE',  ( -28.42127686227592420, -0.6461176296494712812, -221.6028628238154567 ) ) ;
#10625 = CARTESIAN_POINT ( 'NONE',  ( -21.01242583983345469, 16.60754347445175227, -220.8286358486543293 ) ) ;
#10626 = CARTESIAN_POINT ( 'NONE',  ( 0.1645309800062008665, 15.56029994314186382, -233.1129172884685943 ) ) ;
#10627 = CARTESIAN_POINT ( 'NONE',  ( 16.20788843645364352, 6.828976201867700269, -231.6689701909764665 ) ) ;
#10628 = VERTEX_POINT ( 'NONE', #15781 ) ;
#10629 = CARTESIAN_POINT ( 'NONE',  ( 13.43173494629961517, -24.23096015178613172, -223.5315588962966160 ) ) ;
#10630 = AXIS2_PLACEMENT_3D ( 'NONE', #1050, #21628, #6220 ) ;
#10631 = EDGE_LOOP ( 'NONE', ( #16958, #7259 ) ) ;
#10632 = CARTESIAN_POINT ( 'NONE',  ( 13.65368867897269389, -25.84127502057983605, -227.3223880387346867 ) ) ;
#10633 = CARTESIAN_POINT ( 'NONE',  ( -9.060146982536336324, 27.14942986116457746, -225.6568961786626062 ) ) ;
#10634 = ORIENTED_EDGE ( 'NONE', *, *, #20690, .F. ) ;
#10635 = CARTESIAN_POINT ( 'NONE',  ( 0.000000000000000000, 22.63401512838754570, 77.51594804401857175 ) ) ;
#10636 = CARTESIAN_POINT ( 'NONE',  ( 15.12287735332712835, 21.03907941686458116, -231.7894952627153202 ) ) ;
#10637 = CARTESIAN_POINT ( 'NONE',  ( 17.95694455891925756, -3.510678534943489026, -231.2643001502910067 ) ) ;
#10638 = CARTESIAN_POINT ( 'NONE',  ( -20.18470553695442860, -13.13924840112635195, -232.9662461559857718 ) ) ;
#10639 = CARTESIAN_POINT ( 'NONE',  ( 0.04660897052267574947, -31.13860575300111577, -224.7746869833732717 ) ) ;
#10640 = CARTESIAN_POINT ( 'NONE',  ( -1.796846813493219619, 26.08418332695505271, -220.7262848173578504 ) ) ;
#10641 = DIRECTION ( 'NONE',  ( 0.000000000000000000, 1.224646799147472769E-16, 1.000000000000000000 ) ) ;
#10642 = CARTESIAN_POINT ( 'NONE',  ( 14.04819512851487673, 6.831178966487911453, -222.6676118107292552 ) ) ;
#10643 = CARTESIAN_POINT ( 'NONE',  ( -8.501641725227710111, 25.47064987787527102, -217.3358698761548737 ) ) ;
#10644 = CARTESIAN_POINT ( 'NONE',  ( -5.125319492185865577, 20.53749879880200524, -218.7557759432853288 ) ) ;
#10645 = ORIENTED_EDGE ( 'NONE', *, *, #3744, .F. ) ;
#10646 = CARTESIAN_POINT ( 'NONE',  ( 8.175342817246784577, 19.41817470142738244, -216.6818271833384699 ) ) ;
#10647 = CARTESIAN_POINT ( 'NONE',  ( -15.37153448429513602, 5.014568651886798456, -224.5085656291724945 ) ) ;
#10648 = CARTESIAN_POINT ( 'NONE',  ( 28.41961022423218353, 10.76616830294286409, -220.2698681100053193 ) ) ;
#10649 = CARTESIAN_POINT ( 'NONE',  ( 9.759123193367146953, -21.89695672029116480, -217.8292787338521919 ) ) ;
#10651 = CARTESIAN_POINT ( 'NONE',  ( -19.63401512838757057, -1.925929944387226885E-29, 77.51594804401857175 ) ) ;
#10650 = MECHANICAL_DESIGN_GEOMETRIC_PRESENTATION_REPRESENTATION (  '', ( #13170 ), #18199 ) ;
#10652 = ORIENTED_EDGE ( 'NONE', *, *, #7895, .T. ) ;
#10653 = AXIS2_PLACEMENT_3D ( 'NONE', #19150, #17698, #588 ) ;
#10654 = CARTESIAN_POINT ( 'NONE',  ( -6.282398543089500187, 12.01615879894893801, -228.5121145169883903 ) ) ;
#10655 = CARTESIAN_POINT ( 'NONE',  ( 16.72004689093256857, -4.507886829375356008, -228.6412576449023959 ) ) ;
#10656 = DIRECTION ( 'NONE',  ( 0.000000000000000000, 0.000000000000000000, 1.000000000000000000 ) ) ;
#10657 = CARTESIAN_POINT ( 'NONE',  ( 24.03642272140365677, 3.646960756862087205, -218.2320643939070806 ) ) ;
#10658 = CARTESIAN_POINT ( 'NONE',  ( 8.332496243628455090, -29.79192972398156769, -226.1452587264855367 ) ) ;
#10659 = DIRECTION ( 'NONE',  ( 0.000000000000000000, 0.000000000000000000, 1.000000000000000000 ) ) ;
#10660 = CARTESIAN_POINT ( 'NONE',  ( -9.151299407007059017, 9.196974979111923076, -223.9483834032048719 ) ) ;
#10661 = CARTESIAN_POINT ( 'NONE',  ( -12.15711705271618470, 28.08001788883979799, -220.3431297925021681 ) ) ;
#10662 = VERTEX_POINT ( 'NONE', #11343 ) ;
#10663 = CARTESIAN_POINT ( 'NONE',  ( -27.90314475660494153, 12.48829126175061077, -223.3300566725355338 ) ) ;
#10664 = CARTESIAN_POINT ( 'NONE',  ( -17.60306105620566441, -10.62493847279374926, -216.8163279515337649 ) ) ;
#10665 = LINE ( 'NONE', #17530, #4797 ) ;
#10666 = FACE_OUTER_BOUND ( 'NONE', #12207, .T. ) ;
#10667 = CARTESIAN_POINT ( 'NONE',  ( -23.52999999174766543, 19.39566142560855866, -221.9446938626390704 ) ) ;
#10668 = CARTESIAN_POINT ( 'NONE',  ( 0.3555517721839966394, -12.99484957898737569, -222.7951259809431974 ) ) ;
#10669 = CIRCLE ( 'NONE', #19625, 3.000000000000002665 ) ;
#10670 = CARTESIAN_POINT ( 'NONE',  ( 14.75355577798158713, -1.671605614104410886, -222.5078368351397842 ) ) ;
#10671 = CARTESIAN_POINT ( 'NONE',  ( -23.05909213503509392, 9.658626557025268511, -2.611256163095958982 ) ) ;
#10672 = CARTESIAN_POINT ( 'NONE',  ( 15.88536911906737181, 12.85343532334862893, -218.9532478288372204 ) ) ;
#10673 = EDGE_CURVE ( 'NONE', #13837, #21809, #6950, .T. ) ;
#10674 = CARTESIAN_POINT ( 'NONE',  ( -23.66836017558062011, 21.44695383684080525, -223.6245772351065568 ) ) ;
#10675 = DIRECTION ( 'NONE',  ( -1.000000000000000000, -6.982962677686272233E-15, 0.000000000000000000 ) ) ;
#10676 = CARTESIAN_POINT ( 'NONE',  ( 15.99247752609008444, 10.72268246046808216, -230.5614800526110173 ) ) ;
#10677 = CARTESIAN_POINT ( 'NONE',  ( -0.09985864093865706725, -15.05342968659714309, -222.4585048042796132 ) ) ;
#10678 = VERTEX_POINT ( 'NONE', #19659 ) ;
#10679 = PRODUCT_DEFINITION_FORMATION_WITH_SPECIFIED_SOURCE ( 'ANY', '', #13558, .NOT_KNOWN. ) ;
#10680 = CARTESIAN_POINT ( 'NONE',  ( -4.334015487506815312, 18.19775486192265390, -231.4387392399519285 ) ) ;
#10681 = CARTESIAN_POINT ( 'NONE',  ( -16.48883219358909713, 20.84100960965193394, -219.4392138569792507 ) ) ;
#10682 = CARTESIAN_POINT ( 'NONE',  ( -25.98311979368102342, 15.13734258059737670, -220.6162231662327429 ) ) ;
#10683 = CARTESIAN_POINT ( 'NONE',  ( -22.54540532658949914, -16.00113133426942724, -227.3151344909721843 ) ) ;
#10684 = DIRECTION ( 'NONE',  ( -1.000000000000000000, 0.000000000000000000, 0.000000000000000000 ) ) ;
#10685 = EDGE_LOOP ( 'NONE', ( #9870, #19241 ) ) ;
#10686 = CARTESIAN_POINT ( 'NONE',  ( 21.14441169763230732, 12.98245189690719315, -217.0976687089155064 ) ) ;
#10687 = CARTESIAN_POINT ( 'NONE',  ( 5.446054363465077763, -20.62119468428589997, -218.5301445808800622 ) ) ;
#10688 = CARTESIAN_POINT ( 'NONE',  ( 14.39473142419577023, 15.98257177912839389, -217.4557725731239373 ) ) ;
#10689 = CARTESIAN_POINT ( 'NONE',  ( -18.09776816382430908, 23.50806826204562583, -229.9568677523880638 ) ) ;
#10690 = CARTESIAN_POINT ( 'NONE',  ( 13.70863938672594529, 6.616599615120571265, -232.1343637516268643 ) ) ;
#10691 = CARTESIAN_POINT ( 'NONE',  ( 2.539761864897490007, 23.64215977235053501, -233.4645566207487661 ) ) ;
#10692 = CARTESIAN_POINT ( 'NONE',  ( 25.50000000000000000, 0.5000000000000000000, -6.000000000000000000 ) ) ;
#10693 = CARTESIAN_POINT ( 'NONE',  ( -8.514447835183077018, -10.26590951297754195, -225.5321622820681569 ) ) ;
#10694 = CARTESIAN_POINT ( 'NONE',  ( 12.13827923251525220, -9.172799829723585319, -229.1860353116090891 ) ) ;
#10695 = DIRECTION ( 'NONE',  ( -1.000000000000000000, 0.000000000000000000, 0.000000000000000000 ) ) ;
#10696 = FACE_OUTER_BOUND ( 'NONE', #6578, .T. ) ;
#10697 = CARTESIAN_POINT ( 'NONE',  ( -17.81561310496929806, 18.25637658208611569, -215.7745954696244439 ) ) ;
#10698 = CARTESIAN_POINT ( 'NONE',  ( -17.01759357405825668, -4.262369086395770168, -221.2289172648622184 ) ) ;
#10699 = CARTESIAN_POINT ( 'NONE',  ( -16.74094048923576494, 16.03040267675914521, -217.9177456399057178 ) ) ;
#10700 = CARTESIAN_POINT ( 'NONE',  ( 4.303123380281038024, 17.66787810618728827, -231.9745698734655832 ) ) ;
#10701 = CARTESIAN_POINT ( 'NONE',  ( 4.482815116226093188, 26.97722808566452812, -229.2080185206130238 ) ) ;
#10702 = ORIENTED_EDGE ( 'NONE', *, *, #21236, .T. ) ;
#10703 = CARTESIAN_POINT ( 'NONE',  ( 10.74287257054252720, -16.14773823008032849, -215.8883494958819824 ) ) ;
#10704 = ORIENTED_EDGE ( 'NONE', *, *, #9494, .F. ) ;
#10705 = CARTESIAN_POINT ( 'NONE',  ( 14.68783945462866924, 9.535285537539673228, -219.4694094309942045 ) ) ;
#10706 = CARTESIAN_POINT ( 'NONE',  ( -10.83439284573031536, 18.36737820296253432, -234.3014274143859836 ) ) ;
#10707 = CARTESIAN_POINT ( 'NONE',  ( -17.00265675087485917, 7.324244386240115645, -218.5600005870616656 ) ) ;
#10708 = CARTESIAN_POINT ( 'NONE',  ( -22.25980993584449408, -3.522148912989541802, -233.7954546715351398 ) ) ;
#10709 = CARTESIAN_POINT ( 'NONE',  ( -17.75316132689678383, 25.03468689048078843, -222.1645193425721061 ) ) ;
#10710 = CARTESIAN_POINT ( 'NONE',  ( 0.000000000000000000, 0.000000000000000000, -20.00000000000000000 ) ) ;
#10711 = FACE_OUTER_BOUND ( 'NONE', #15390, .T. ) ;
#10712 = CARTESIAN_POINT ( 'NONE',  ( 27.79746884017060538, 13.63637251724950339, -226.5788410723774575 ) ) ;
#10713 = CARTESIAN_POINT ( 'NONE',  ( -22.53796032816233463, 16.84148256071415872, -226.0516062466300582 ) ) ;
#10714 = CARTESIAN_POINT ( 'NONE',  ( 10.00603923119254723, 9.610873433734882454, -231.2388095806506669 ) ) ;
#10715 = CARTESIAN_POINT ( 'NONE',  ( 28.09488075336259527, 3.911739131332936381, -227.7543364642411632 ) ) ;
#10716 = CARTESIAN_POINT ( 'NONE',  ( -30.74480097515601074, -10.13586512673612106, -225.7096819839593707 ) ) ;
#10717 = CARTESIAN_POINT ( 'NONE',  ( -21.50522087930578152, -16.03150550247721640, -231.4768288373508369 ) ) ;
#10718 = CARTESIAN_POINT ( 'NONE',  ( -23.70973587455150522, 20.45398817402440983, -228.9005348699235469 ) ) ;
#10719 = CARTESIAN_POINT ( 'NONE',  ( -15.62091161899253855, -26.00636881980398840, -222.1463585103649905 ) ) ;
#10720 = CARTESIAN_POINT ( 'NONE',  ( 18.29617186523616468, 23.20920553663278341, -223.4372550713720216 ) ) ;
#10721 = CARTESIAN_POINT ( 'NONE',  ( 15.13450096816097634, -26.20215934980152639, -231.3023426574493726 ) ) ;
#10722 = DIRECTION ( 'NONE',  ( -1.000000000000000000, 0.000000000000000000, 0.000000000000000000 ) ) ;
#10723 = CARTESIAN_POINT ( 'NONE',  ( 22.16327814861754675, 7.634676377199016706, -234.0520676664821735 ) ) ;
#10724 = PRESENTATION_STYLE_ASSIGNMENT (( #17813 ) ) ;
#10725 = CARTESIAN_POINT ( 'NONE',  ( -2.554014161526931392, 17.56271496069470572, -229.4905841158208659 ) ) ;
#10726 = CARTESIAN_POINT ( 'NONE',  ( -18.04772061096520375, 5.916925414182395038, -217.8829197293425750 ) ) ;
#10727 = CARTESIAN_POINT ( 'NONE',  ( 15.05360126642391450, 1.481754003466396963, -222.9454997252120734 ) ) ;
#10728 = CARTESIAN_POINT ( 'NONE',  ( 16.43556216695724004, 8.397919695511960825, -216.7971521583719152 ) ) ;
#10729 = CARTESIAN_POINT ( 'NONE',  ( -10.96310611394154755, -12.59072721579616605, -220.6792497830813318 ) ) ;
#10730 = CARTESIAN_POINT ( 'NONE',  ( 5.179557175392591972, 10.46258103618983881, -224.6216839350439614 ) ) ;
#10731 = CARTESIAN_POINT ( 'NONE',  ( 26.00000000000000000, 4.399999999999999467, -3.300000000000000266 ) ) ;
#10732 = CARTESIAN_POINT ( 'NONE',  ( -9.037518995728490268, -13.81466884781966620, -216.3195389756191673 ) ) ;
#10733 = CARTESIAN_POINT ( 'NONE',  ( -4.170472558179216804, 16.67407401355319152, -230.2690496885289804 ) ) ;
#10734 = CARTESIAN_POINT ( 'NONE',  ( 13.20340559785743828, 9.575208899273587093, -218.1210831379648312 ) ) ;
#10735 = CARTESIAN_POINT ( 'NONE',  ( -17.55809605150417951, 6.636094600389130349, -229.8856864643722986 ) ) ;
#10736 = CIRCLE ( 'NONE', #2452, 2.000000000000001776 ) ;
#10737 = CARTESIAN_POINT ( 'NONE',  ( -12.15711705271618470, 28.08001788883979799, -220.3431297925021681 ) ) ;
#10738 = CARTESIAN_POINT ( 'NONE',  ( 13.15438416660314225, 5.520603777723624539, -227.0878346348094681 ) ) ;
#10739 = CARTESIAN_POINT ( 'NONE',  ( 8.290903921942224031, -23.90349455650518351, -230.1727405421096364 ) ) ;
#10740 = ORIENTED_EDGE ( 'NONE', *, *, #13487, .F. ) ;
#10741 = CARTESIAN_POINT ( 'NONE',  ( 10.52067862919218832, -10.34113464825721351, -228.4460540958991714 ) ) ;
#10742 = CARTESIAN_POINT ( 'NONE',  ( -8.881241380679488984, 27.18697625135247975, -224.4474391433207927 ) ) ;
#10743 = ORIENTED_EDGE ( 'NONE', *, *, #4856, .F. ) ;
#10744 = CARTESIAN_POINT ( 'NONE',  ( 10.50530447320976535, 20.19629329636330084, -217.1354359361034767 ) ) ;
#10745 = CARTESIAN_POINT ( 'NONE',  ( -25.32359575169976296, -0.6821277435459325300, -233.2512658769913969 ) ) ;
#10746 = CARTESIAN_POINT ( 'NONE',  ( -11.88525712185471050, -8.925198460467992589, -221.0951487055306472 ) ) ;
#10747 = CARTESIAN_POINT ( 'NONE',  ( -6.642805165258356404, -28.12267032419628521, -230.9452027245340560 ) ) ;
#10748 = CARTESIAN_POINT ( 'NONE',  ( -5.560972518124746244, 14.60655266358653215, -227.5460946431043681 ) ) ;
#10749 = CARTESIAN_POINT ( 'NONE',  ( 0.000000000000000000, 21.63401512838747820, 77.51594804401857175 ) ) ;
#10750 = CARTESIAN_POINT ( 'NONE',  ( 23.24653631066306048, 11.83805845626388020, -219.6020901153134162 ) ) ;
#10751 = CARTESIAN_POINT ( 'NONE',  ( -6.201839134465864767, 11.37481922992157379, -223.7040893475979146 ) ) ;
#10752 = CARTESIAN_POINT ( 'NONE',  ( -8.112279890008961658, 11.99566605360304727, -225.9834628568286519 ) ) ;
#10753 = ORIENTED_EDGE ( 'NONE', *, *, #9879, .T. ) ;
#10754 = EDGE_CURVE ( 'NONE', #18119, #580, #12703, .T. ) ;
#10755 = CARTESIAN_POINT ( 'NONE',  ( -1.301562195391901877, 16.19210386685474390, -220.0867867038183192 ) ) ;
#10756 = CARTESIAN_POINT ( 'NONE',  ( -18.42638600874552424, 7.060399206045774534, -230.3991437614443214 ) ) ;
#10757 = CARTESIAN_POINT ( 'NONE',  ( 17.85905871012913693, 8.463974683125162102, -234.6532732619751300 ) ) ;
#10758 = CARTESIAN_POINT ( 'NONE',  ( 9.037704487505543227, -20.74919929927824214, -217.6023494967207625 ) ) ;
#10759 = LINE ( 'NONE', #17624, #7503 ) ;
#10760 = DIRECTION ( 'NONE',  ( -1.000000000000000000, 0.000000000000000000, 0.000000000000000000 ) ) ;
#10761 = CARTESIAN_POINT ( 'NONE',  ( 8.496844655769807630, 14.66037471857024599, -219.1631158796573118 ) ) ;
#10762 = CARTESIAN_POINT ( 'NONE',  ( 26.31881739696682843, -8.664992621510689830, -226.4435203923285655 ) ) ;
#10763 = DIRECTION ( 'NONE',  ( 0.000000000000000000, 0.000000000000000000, 1.000000000000000000 ) ) ;
#10764 = CARTESIAN_POINT ( 'NONE',  ( 17.07668571305246985, 2.037405138410691485, -219.7626854147787867 ) ) ;
#10765 = CARTESIAN_POINT ( 'NONE',  ( 1.752757082432757185, -17.15725705531007250, -232.7539178101738742 ) ) ;
#10766 = CARTESIAN_POINT ( 'NONE',  ( -11.49049084071896409, 11.06834963248926940, -218.3354249205727058 ) ) ;
#10767 = CARTESIAN_POINT ( 'NONE',  ( -19.98042543492610079, 23.51949599776966693, -226.6701036947414138 ) ) ;
#10768 = CARTESIAN_POINT ( 'NONE',  ( -14.70651859537745487, 4.211702956367679107, -230.0357207626005334 ) ) ;
#10769 = CARTESIAN_POINT ( 'NONE',  ( -19.43452863239301820, -21.19996443032342626, -221.1427059245750399 ) ) ;
#10770 = DIRECTION ( 'NONE',  ( -0.000000000000000000, -1.000000000000000000, -0.000000000000000000 ) ) ;
#10771 = CARTESIAN_POINT ( 'NONE',  ( -23.00000000000000000, -1.421401133463427911E-20, 10.00000000000000000 ) ) ;
#10772 = CARTESIAN_POINT ( 'NONE',  ( -22.99617382825321599, 17.18101613848176967, -230.9512687019100099 ) ) ;
#10773 = CARTESIAN_POINT ( 'NONE',  ( 7.808093059109005196, -25.57408461116448706, -218.1679985877120487 ) ) ;
#10774 = DIRECTION ( 'NONE',  ( 6.982962677686266711E-15, -1.000000000000000000, 0.000000000000000000 ) ) ;
#10775 = CARTESIAN_POINT ( 'NONE',  ( 18.51425713624010427, 11.82474821235740592, -231.3645840199355632 ) ) ;
#10776 = CARTESIAN_POINT ( 'NONE',  ( -8.653738780971721667, 11.12943719949617893, -219.7525355316396087 ) ) ;
#10777 = DIRECTION ( 'NONE',  ( 0.000000000000000000, 0.000000000000000000, -1.000000000000000000 ) ) ;
#10778 = CARTESIAN_POINT ( 'NONE',  ( 19.67070349224072956, 16.44307963282299312, -220.0378483479504439 ) ) ;
#10779 = CARTESIAN_POINT ( 'NONE',  ( 3.098311947274309919, -13.44192016451707872, -223.0038505953381502 ) ) ;
#10780 = EDGE_CURVE ( 'NONE', #20645, #21551, #8753, .T. ) ;
#10781 = EDGE_LOOP ( 'NONE', ( #9737, #19755, #12772, #2137 ) ) ;
#10782 = CARTESIAN_POINT ( 'NONE',  ( -4.466732464217805898, 19.42663028452474450, -231.9485309169485561 ) ) ;
#10783 = CARTESIAN_POINT ( 'NONE',  ( -15.07599795178976443, 12.40109266655585429, -218.9921934537110815 ) ) ;
#10784 = CARTESIAN_POINT ( 'NONE',  ( -14.83095329101371540, 1.580869236763225549, -217.8331819987577660 ) ) ;
#10785 = EDGE_LOOP ( 'NONE', ( #13954, #13523, #11446, #19220 ) ) ;
#10786 = CARTESIAN_POINT ( 'NONE',  ( -13.53417258903678722, -8.044363197357762729, -224.1542709308240546 ) ) ;
#10787 = CARTESIAN_POINT ( 'NONE',  ( 0.000000000000000000, 0.000000000000000000, -75.00000000000000000 ) ) ;
#10788 = ORIENTED_EDGE ( 'NONE', *, *, #17641, .T. ) ;
#10789 = CARTESIAN_POINT ( 'NONE',  ( 17.89221702206198117, 0.2742047965568425449, -220.2420650470893122 ) ) ;
#10790 = CARTESIAN_POINT ( 'NONE',  ( 2.737864789122675280, -26.51934750686404385, -230.0373452194950517 ) ) ;
#10791 = CARTESIAN_POINT ( 'NONE',  ( 18.04365516558436866, 6.721233635139160612, -218.4376093631473168 ) ) ;
#10792 = CARTESIAN_POINT ( 'NONE',  ( -3.501680520304516264, 14.31538576447642264, -219.8967178229432307 ) ) ;
#10793 = ADVANCED_FACE ( 'NONE', ( #2555 ), #16298, .T. ) ;
#10794 = CARTESIAN_POINT ( 'NONE',  ( 25.70350299105564318, 4.008313962570879241, -233.1578316763087173 ) ) ;
#10795 = CARTESIAN_POINT ( 'NONE',  ( 8.689059922489732912, 15.18271246186214363, -218.7354841152034908 ) ) ;
#10796 = CARTESIAN_POINT ( 'NONE',  ( -21.63401512838757768, 0.000000000000000000, 77.51594804401857175 ) ) ;
#10797 = ADVANCED_FACE ( 'NONE', ( #10711 ), #13063, .F. ) ;
#10798 = CARTESIAN_POINT ( 'NONE',  ( -18.44715843167851688, -19.86029123650958184, -231.9563062773970046 ) ) ;
#10799 = CARTESIAN_POINT ( 'NONE',  ( 15.50779141722566656, -5.694711448414747856, -219.6385356284298211 ) ) ;
#10800 = CARTESIAN_POINT ( 'NONE',  ( 24.63401512838761320, 0.000000000000000000, 77.51594804401857175 ) ) ;
#10801 = CARTESIAN_POINT ( 'NONE',  ( -21.73153953336191790, 8.758376218440917071, -235.2971293019126051 ) ) ;
#10802 = CARTESIAN_POINT ( 'NONE',  ( -21.44067990442788840, -11.35877574734454143, -219.4569350636155605 ) ) ;
#10803 = CARTESIAN_POINT ( 'NONE',  ( -13.96147744945181124, 5.260363697127891314, -222.3342733685200301 ) ) ;
#10804 = CARTESIAN_POINT ( 'NONE',  ( 16.55626903245587656, 22.80423546114836952, -218.9884947126587633 ) ) ;
#10805 = CARTESIAN_POINT ( 'NONE',  ( 5.585286719045844173, 27.51657303716567426, -222.4190945945824751 ) ) ;
#10806 = EDGE_LOOP ( 'NONE', ( #2068, #8576 ) ) ;
#10807 = CARTESIAN_POINT ( 'NONE',  ( 22.41656803062015157, -8.700679067278056067, -214.8043567724421337 ) ) ;
#10808 = ORIENTED_EDGE ( 'NONE', *, *, #17805, .F. ) ;
#10809 = CARTESIAN_POINT ( 'NONE',  ( 28.57344184061583192, 5.631897254180425527, -225.1192013637692355 ) ) ;
#10810 = CARTESIAN_POINT ( 'NONE',  ( -18.41237742040652847, 14.06446039901721790, -216.7469276929859632 ) ) ;
#10811 = CARTESIAN_POINT ( 'NONE',  ( -13.41298582792616934, 27.85383138489214616, -228.6457525465575884 ) ) ;
#10812 = CARTESIAN_POINT ( 'NONE',  ( -13.68337831708448782, -3.656824064325736590, -221.3737413816871538 ) ) ;
#10813 = CARTESIAN_POINT ( 'NONE',  ( -13.56774755469388616, 7.311522441667196226, -219.1912666243428021 ) ) ;
#10814 = DIRECTION ( 'NONE',  ( 0.000000000000000000, 0.000000000000000000, -1.000000000000000000 ) ) ;
#10815 = AXIS2_PLACEMENT_3D ( 'NONE', #731, #9402, #9516 ) ;
#10816 = CARTESIAN_POINT ( 'NONE',  ( 16.08921376350389920, -2.840750994787607731, -229.5571464835293796 ) ) ;
#10817 = CARTESIAN_POINT ( 'NONE',  ( -14.46024998630872282, 14.54669730493860946, -231.4156670963686508 ) ) ;
#10818 = CARTESIAN_POINT ( 'NONE',  ( 28.41961022423218353, 10.76616830294286409, -220.2698681100053193 ) ) ;
#10819 = CARTESIAN_POINT ( 'NONE',  ( -29.88125065636863198, 4.504452993877526623, -226.2048141718237275 ) ) ;
#10820 = CARTESIAN_POINT ( 'NONE',  ( 10.57926812561479757, 10.00910231482511215, -225.8341706491384286 ) ) ;
#10821 = CARTESIAN_POINT ( 'NONE',  ( -14.28784611495131784, -7.281039336628973402, -230.6208668958216208 ) ) ;
#10822 = CARTESIAN_POINT ( 'NONE',  ( 5.720314275582434327, 25.17872937134267630, -219.7530083620574430 ) ) ;
#10823 = CARTESIAN_POINT ( 'NONE',  ( -4.670971249126254499, -22.80666086768999890, -234.0323572959307512 ) ) ;
#10824 = CARTESIAN_POINT ( 'NONE',  ( 11.33210854356620523, 22.81476816607802149, -217.8536224460118262 ) ) ;
#10825 = CARTESIAN_POINT ( 'NONE',  ( 7.844578353157877437, -11.10597526584381356, -230.9016046914076128 ) ) ;
#10826 = CARTESIAN_POINT ( 'NONE',  ( -14.57944476639264764, 6.129437248167259433, -229.4766146696829310 ) ) ;
#10827 = CARTESIAN_POINT ( 'NONE',  ( 0.000000000000000000, 0.000000000000000000, 75.00000000000000000 ) ) ;
#10828 = CARTESIAN_POINT ( 'NONE',  ( -28.68324149884075780, -4.473022182960058934, -227.9839418391680681 ) ) ;
#10829 = CARTESIAN_POINT ( 'NONE',  ( 3.755404788550845474, 24.96758616565139022, -220.0839658302907935 ) ) ;
#10830 = CARTESIAN_POINT ( 'NONE',  ( -21.19360951076126653, 12.15251088906093457, -217.9482185194656552 ) ) ;
#10831 = CARTESIAN_POINT ( 'NONE',  ( 22.66390650824515873, 11.48342577402021725, -231.3155567808436217 ) ) ;
#10832 = CARTESIAN_POINT ( 'NONE',  ( -11.81856518996410088, -14.35937779267807279, -219.1576658967449305 ) ) ;
#10833 = CARTESIAN_POINT ( 'NONE',  ( 15.51445714770079931, 9.275596138242290678, -215.8565574371285436 ) ) ;
#10834 = CARTESIAN_POINT ( 'NONE',  ( 0.000000000000000000, 0.000000000000000000, 60.00000000000001421 ) ) ;
#10835 = CARTESIAN_POINT ( 'NONE',  ( -4.051702682916754839, -14.52120462818199798, -217.8402208339018671 ) ) ;
#10836 = CARTESIAN_POINT ( 'NONE',  ( -9.627017372966443887, 15.60690227900018279, -218.8878023709062859 ) ) ;
#10837 = CARTESIAN_POINT ( 'NONE',  ( 17.97920459523930958, 17.43922474653955490, -233.2737719749805763 ) ) ;
#10838 = AXIS2_PLACEMENT_3D ( 'NONE', #11635, #4648, #15133 ) ;
#10839 = CARTESIAN_POINT ( 'NONE',  ( -25.20870746202117729, 11.68425842440532136, -223.9066764530103342 ) ) ;
#10840 = CARTESIAN_POINT ( 'NONE',  ( 0.6332696906856497554, 18.74964962670039625, -234.8596399859513042 ) ) ;
#10841 = CARTESIAN_POINT ( 'NONE',  ( 17.28149325064817887, -1.074788064772476792, -229.5315781944399305 ) ) ;
#10842 = CARTESIAN_POINT ( 'NONE',  ( 11.82295278175540787, -22.41907685134884076, -220.1071383070178342 ) ) ;
#10843 = CARTESIAN_POINT ( 'NONE',  ( 9.020349274477036161, -13.22217574948208529, -220.4173403795374213 ) ) ;
#10844 = CARTESIAN_POINT ( 'NONE',  ( 0.6289891638115701067, 16.47510600144228832, -227.0521699048171342 ) ) ;
#10845 = DIRECTION ( 'NONE',  ( 4.845403715540905824E-30, -6.938893903907257960E-16, -1.000000000000000000 ) ) ;
#10846 = AXIS2_PLACEMENT_3D ( 'NONE', #6011, #16373, #20062 ) ;
#10847 = CARTESIAN_POINT ( 'NONE',  ( 18.54610009393809023, 0.6523581019769808531, -231.1787333216317677 ) ) ;
#10848 = CARTESIAN_POINT ( 'NONE',  ( -14.27185570462694919, -0.4134134650712557035, -229.5903738612280449 ) ) ;
#10849 = CARTESIAN_POINT ( 'NONE',  ( -8.514447835183077018, -10.26590951297754195, -225.5321622820681569 ) ) ;
#10850 = CARTESIAN_POINT ( 'NONE',  ( 2.513843158659109456, -14.78137297724497401, -219.3443999184743518 ) ) ;
#10851 = CARTESIAN_POINT ( 'NONE',  ( -2.532302712337851425, 16.54370602006230939, -228.1940632970506613 ) ) ;
#10852 = FACE_OUTER_BOUND ( 'NONE', #6919, .T. ) ;
#10853 = CARTESIAN_POINT ( 'NONE',  ( -12.12559971566433958, 1.856299769312002912, -227.8748781050665286 ) ) ;
#10854 = CARTESIAN_POINT ( 'NONE',  ( -2.735889804569492600, 12.71735652435744512, -225.1194195722198117 ) ) ;
#10855 = CARTESIAN_POINT ( 'NONE',  ( 0.04449911090679885967, 16.51968908208873899, -222.9067194156212111 ) ) ;
#10856 = EDGE_LOOP ( 'NONE', ( #14828, #8865, #3417, #11068 ) ) ;
#10857 = CIRCLE ( 'NONE', #2170, 9.000000000000001776 ) ;
#10858 = CARTESIAN_POINT ( 'NONE',  ( -3.223980134944351317, 26.83284996841001302, -219.5167893230652965 ) ) ;
#10859 = CARTESIAN_POINT ( 'NONE',  ( 20.13946171159960841, -0.1427001808266660232, -233.7987036390019853 ) ) ;
#10860 = CARTESIAN_POINT ( 'NONE',  ( 16.77642802340811556, -0.6192566135115280535, -218.8326447441449432 ) ) ;
#10861 = CARTESIAN_POINT ( 'NONE',  ( 7.640685522499278903, -12.22373526560700441, -226.1755943870604710 ) ) ;
#10862 = LINE ( 'NONE', #12336, #2105 ) ;
#10863 = DIRECTION ( 'NONE',  ( 0.1093404791528972547, -0.9940043559354329039, 0.000000000000000000 ) ) ;
#10864 = ADVANCED_FACE ( 'NONE', ( #246 ), #7672, .T. ) ;
#10865 = CARTESIAN_POINT ( 'NONE',  ( 5.623554730548537606, 15.65270319720736225, -231.3185741195121068 ) ) ;
#10866 = CARTESIAN_POINT ( 'NONE',  ( 20.55466028792283240, -8.067975053177056211, -219.1472888552992799 ) ) ;
#10867 = CARTESIAN_POINT ( 'NONE',  ( 17.95451841861686049, -2.630205674513758549E-15, -101.2940952255125922 ) ) ;
#10868 = CIRCLE ( 'NONE', #17702, 25.00000000000000355 ) ;
#10869 = CARTESIAN_POINT ( 'NONE',  ( 7.486336813247038258, -29.35413437595724773, -221.4114973598149447 ) ) ;
#10870 = CARTESIAN_POINT ( 'NONE',  ( -11.33137429837660193, 27.25022425932026238, -230.1650924901870212 ) ) ;
#10871 = CARTESIAN_POINT ( 'NONE',  ( -10.33514150881494942, 13.62639309082336503, -216.9544063991933172 ) ) ;
#10872 = ORIENTED_EDGE ( 'NONE', *, *, #21188, .T. ) ;
#10873 = CARTESIAN_POINT ( 'NONE',  ( -7.395406416482832590, 12.93623984139929739, -219.2606224730616873 ) ) ;
#10874 = CARTESIAN_POINT ( 'NONE',  ( -10.39692419770002552, -10.11462123336039021, -222.6538761800393047 ) ) ;
#10875 = CARTESIAN_POINT ( 'NONE',  ( 0.000000000000000000, 23.00000000000000000, -60.00000000000000000 ) ) ;
#10876 = CARTESIAN_POINT ( 'NONE',  ( -9.740348021262962064, 16.12529029871877384, -216.4361617420699702 ) ) ;
#10877 = CARTESIAN_POINT ( 'NONE',  ( 9.552164729858477088, -28.54380927792562872, -224.2925619065192677 ) ) ;
#10878 = AXIS2_PLACEMENT_3D ( 'NONE', #3517, #7137, #22209 ) ;
#10879 = FILL_AREA_STYLE ('',( #3897 ) ) ;
#10880 = CARTESIAN_POINT ( 'NONE',  ( -17.79285498209129202, 9.187865686019035749, -216.3798185811636756 ) ) ;
#10881 = AXIS2_PLACEMENT_3D ( 'NONE', #4499, #686, #14429 ) ;
#10882 = CARTESIAN_POINT ( 'NONE',  ( 15.54095364727189299, 10.52000078266145700, -230.2714373371992735 ) ) ;
#10883 = CARTESIAN_POINT ( 'NONE',  ( -11.23881320317003407, 15.84151802331611236, -234.2799649731619809 ) ) ;
#10884 = CARTESIAN_POINT ( 'NONE',  ( -22.00000000000001421, 0.000000000000000000, -224.9999999999999716 ) ) ;
#10885 = CARTESIAN_POINT ( 'NONE',  ( 16.07044873961816123, 22.39643131523411412, -226.8512752114033901 ) ) ;
#10886 = CARTESIAN_POINT ( 'NONE',  ( -6.954422770286640798, -15.70181985945210634, -221.3390676453758488 ) ) ;
#10887 = VERTEX_POINT ( 'NONE', #16191 ) ;
#10888 = CARTESIAN_POINT ( 'NONE',  ( 2.808299412262623473, 18.06245856371233316, -217.9832661743849656 ) ) ;
#10889 = CARTESIAN_POINT ( 'NONE',  ( -13.14888680331901583, 26.03314517226533908, -227.7900104434697539 ) ) ;
#10890 = CARTESIAN_POINT ( 'NONE',  ( -16.65220264499505376, 11.77543314451157563, -216.3149620944649030 ) ) ;
#10891 = ORIENTED_EDGE ( 'NONE', *, *, #11148, .F. ) ;
#10892 = CARTESIAN_POINT ( 'NONE',  ( -19.48378335617362112, -12.36282430725977655, -218.8185104403611945 ) ) ;
#10893 = DIRECTION ( 'NONE',  ( 0.000000000000000000, 0.000000000000000000, -1.000000000000000000 ) ) ;
#10894 = EDGE_LOOP ( 'NONE', ( #4738, #22182, #16166, #22005 ) ) ;
#10895 = CARTESIAN_POINT ( 'NONE',  ( -13.92046207272054303, -0.1600067567908077248, -224.5811699126800818 ) ) ;
#10896 = CARTESIAN_POINT ( 'NONE',  ( 6.772180301198498675, -16.47206380092378097, -229.1778777248402719 ) ) ;
#10897 = CARTESIAN_POINT ( 'NONE',  ( 15.76910524310159900, 5.601482066865847820, -220.3440822020379528 ) ) ;
#10898 = CARTESIAN_POINT ( 'NONE',  ( -1.881996891245037995, 28.05344686410985489, -218.6379207300106202 ) ) ;
#10899 = AXIS2_PLACEMENT_3D ( 'NONE', #6542, #12064, #13413 ) ;
#10900 = CONICAL_SURFACE ( 'NONE', #3688, 25.00000000000000000, 0.1745329251994333364 ) ;
#10901 = CARTESIAN_POINT ( 'NONE',  ( -17.59913672443795463, -0.5356773789333074687, -220.7342471185320960 ) ) ;
#10902 = ADVANCED_FACE ( 'NONE', ( #763 ), #20819, .F. ) ;
#10903 = CARTESIAN_POINT ( 'NONE',  ( 24.34047711160105720, 17.90454708687460794, -228.1939002122307159 ) ) ;
#10904 = CARTESIAN_POINT ( 'NONE',  ( 18.50911814746675788, 15.92944434255054453, -232.0449215596906072 ) ) ;
#10905 = LINE ( 'NONE', #9113, #18463 ) ;
#10906 = CARTESIAN_POINT ( 'NONE',  ( -11.28700884291539630, -21.85791790461604478, -233.5354093188319951 ) ) ;
#10907 = CARTESIAN_POINT ( 'NONE',  ( 4.682724365302521896, -22.35092628325669750, -215.9543778044225348 ) ) ;
#10908 = DIRECTION ( 'NONE',  ( -0.000000000000000000, -0.000000000000000000, -1.000000000000000000 ) ) ;
#10909 = CARTESIAN_POINT ( 'NONE',  ( 0.000000000000000000, 0.000000000000000000, -77.51594804401857175 ) ) ;
#10910 = CARTESIAN_POINT ( 'NONE',  ( -7.329856113536736828, 10.17606210583481818, -226.3085553030691415 ) ) ;
#10911 = CARTESIAN_POINT ( 'NONE',  ( -15.83567870103663466, -7.501751145129069265, -221.2716155488439824 ) ) ;
#10912 = AXIS2_PLACEMENT_3D ( 'NONE', #14516, #21238, #6052 ) ;
#10913 = CIRCLE ( 'NONE', #13798, 17.50000000000000711 ) ;
#10914 = EDGE_CURVE ( 'NONE', #3468, #8526, #13416, .T. ) ;
#10915 = CARTESIAN_POINT ( 'NONE',  ( -19.65084584916038324, 18.01805631773661176, -219.5040736310571106 ) ) ;
#10916 = CARTESIAN_POINT ( 'NONE',  ( 11.01659168199870287, 19.17922986229587323, -233.3715978632214387 ) ) ;
#10917 = CARTESIAN_POINT ( 'NONE',  ( 0.7903203334012884884, 21.30772501796948859, -217.9064416298261619 ) ) ;
#10918 = ORIENTED_EDGE ( 'NONE', *, *, #9143, .T. ) ;
#10919 = CARTESIAN_POINT ( 'NONE',  ( 17.65733440236621732, -13.95165017647719452, -214.8231966952668301 ) ) ;
#10920 = CARTESIAN_POINT ( 'NONE',  ( 15.52719855059926424, 1.633696074270991172, -221.7349885876216433 ) ) ;
#10921 = CARTESIAN_POINT ( 'NONE',  ( 1.557078628722260438, 24.20011951319323273, -235.1441088220640268 ) ) ;
#10922 = CARTESIAN_POINT ( 'NONE',  ( -19.27153818831731158, 23.75761453444584248, -221.9111479746408975 ) ) ;
#10923 = CARTESIAN_POINT ( 'NONE',  ( -29.90835019730369737, -3.078401082523886334, -228.7630230812432046 ) ) ;
#10924 = CARTESIAN_POINT ( 'NONE',  ( -23.98802705797876200, 19.46654170242919690, -223.5293093576406989 ) ) ;
#10925 = DIRECTION ( 'NONE',  ( -0.000000000000000000, -0.000000000000000000, -1.000000000000000000 ) ) ;
#10926 = CARTESIAN_POINT ( 'NONE',  ( 16.50235023187294203, -3.000022380394500310, -230.0447763498268614 ) ) ;
#10927 = AXIS2_PLACEMENT_3D ( 'NONE', #4469, #11350, #18220 ) ;
#10928 = CARTESIAN_POINT ( 'NONE',  ( -4.974038791218384326, 28.61915055369004079, -219.5057940952933961 ) ) ;
#10929 = CARTESIAN_POINT ( 'NONE',  ( 21.75737151495493649, -2.205713500382455283, -233.2756072794337285 ) ) ;
#10930 = CARTESIAN_POINT ( 'NONE',  ( -20.26851768784797869, -0.8260594303982465858, -217.1279713726092098 ) ) ;
#10931 = CIRCLE ( 'NONE', #17414, 25.00000000000000355 ) ;
#10932 = CARTESIAN_POINT ( 'NONE',  ( 11.62313423782632782, 11.98467543564608029, -219.7293303032897995 ) ) ;
#10933 = CARTESIAN_POINT ( 'NONE',  ( -22.54883021006152433, -16.50439104605484530, -230.5104955902558004 ) ) ;
#10934 = CARTESIAN_POINT ( 'NONE',  ( -1.582540545905128049, 14.52388882916313584, -222.9138157219475147 ) ) ;
#10935 = CARTESIAN_POINT ( 'NONE',  ( -7.800954605602409053, -29.95157606033723496, -226.5906573908930000 ) ) ;
#10936 = CARTESIAN_POINT ( 'NONE',  ( 7.995304978256253747, 13.28024228361502779, -220.6535174700288451 ) ) ;
#10937 = CARTESIAN_POINT ( 'NONE',  ( 4.956111054478943068, -16.91316901532391270, -234.1076498343193748 ) ) ;
#10938 = CARTESIAN_POINT ( 'NONE',  ( -23.06814834742187514, 0.000000000000000000, -74.48236190979496030 ) ) ;
#10939 = CARTESIAN_POINT ( 'NONE',  ( -17.49393085256189906, 10.63366922396483361, -217.7502683347138657 ) ) ;
#10940 = SURFACE_STYLE_FILL_AREA ( #5534 ) ;
#10941 = CARTESIAN_POINT ( 'NONE',  ( -22.16366393984728234, -4.852915104599624385, -232.2864540303542924 ) ) ;
#10942 = ADVANCED_FACE ( 'NONE', ( #3713 ), #14867, .F. ) ;
#10943 = CARTESIAN_POINT ( 'NONE',  ( 4.152856881432678726, 16.71326706899027670, -228.3712188091315909 ) ) ;
#10944 = CARTESIAN_POINT ( 'NONE',  ( -23.20103936322198024, 10.64725167743880085, -231.7714206262400864 ) ) ;
#10945 = CARTESIAN_POINT ( 'NONE',  ( 15.61962121506769385, 4.525360868525488911, -229.0684696061408090 ) ) ;
#10946 = CARTESIAN_POINT ( 'NONE',  ( -20.23770393675990675, -19.63250941609856426, -227.7987059506201319 ) ) ;
#10947 = CARTESIAN_POINT ( 'NONE',  ( 23.07558131619435571, 16.33594519118144817, -217.0553921114837124 ) ) ;
#10948 = CIRCLE ( 'NONE', #169, 3.000000000000002665 ) ;
#10949 = CARTESIAN_POINT ( 'NONE',  ( 0.000000000000000000, 0.000000000000000000, 90.00000000000000000 ) ) ;
#10950 = CARTESIAN_POINT ( 'NONE',  ( -18.70843642779997040, -17.48186590846855992, -215.2841814587906981 ) ) ;
#10951 = CARTESIAN_POINT ( 'NONE',  ( 10.40160332990717151, 27.59713857063802323, -221.5374724512453213 ) ) ;
#10952 = CARTESIAN_POINT ( 'NONE',  ( 19.40629804599390340, 15.10110417999774057, -216.3942729496570223 ) ) ;
#10953 = CARTESIAN_POINT ( 'NONE',  ( -11.69222874857179484, 25.57550432052970280, -219.9467848335519591 ) ) ;
#10954 = CARTESIAN_POINT ( 'NONE',  ( -8.995433708001568718, 13.44373928221519243, -231.9251680978426577 ) ) ;
#10955 = CARTESIAN_POINT ( 'NONE',  ( 21.83031488337932657, -1.542591969257240070, -231.3901500139511427 ) ) ;
#10956 = ORIENTED_EDGE ( 'NONE', *, *, #4003, .T. ) ;
#10957 = CARTESIAN_POINT ( 'NONE',  ( 14.94332666820587008, -17.95933738324940165, -219.3037465242801147 ) ) ;
#10958 = ORIENTED_EDGE ( 'NONE', *, *, #3078, .T. ) ;
#10959 = CARTESIAN_POINT ( 'NONE',  ( 10.73531068932428667, -10.59494929936097307, -229.0901643129046192 ) ) ;
#10960 = VERTEX_POINT ( 'NONE', #17466 ) ;
#10961 = CARTESIAN_POINT ( 'NONE',  ( 25.50000000000000000, -3.600000000000001421, -2.699999999999999289 ) ) ;
#10962 = CARTESIAN_POINT ( 'NONE',  ( -21.89065952084861522, -0.9940043559354512226, -215.0000000000000000 ) ) ;
#10963 = CARTESIAN_POINT ( 'NONE',  ( -13.58432508418311180, -0.3977623232610293935, -228.1278904906119465 ) ) ;
#10964 = CARTESIAN_POINT ( 'NONE',  ( -25.61235545225478560, -15.41032726095661509, -226.9890212492312855 ) ) ;
#10965 = CARTESIAN_POINT ( 'NONE',  ( -1.308474130992312023, -24.58654860180777391, -216.2430112183533026 ) ) ;
#10966 = AXIS2_PLACEMENT_3D ( 'NONE', #305, #19308, #77 ) ;
#10967 = CARTESIAN_POINT ( 'NONE',  ( 8.632180352507942800, 16.83956698119041917, -230.4752415867875186 ) ) ;
#10968 = CARTESIAN_POINT ( 'NONE',  ( 0.000000000000000000, 0.000000000000000000, 75.00000000000000000 ) ) ;
#10969 = CARTESIAN_POINT ( 'NONE',  ( -31.04267853410473421, 7.029517189377418873, -226.8060334161593516 ) ) ;
#10970 = CARTESIAN_POINT ( 'NONE',  ( -3.205260335674071648, 17.52234722004434531, -232.9754319808710363 ) ) ;
#10971 = CARTESIAN_POINT ( 'NONE',  ( 2.021807401899061496, 24.17554150923399092, -230.4042646614662146 ) ) ;
#10972 = CARTESIAN_POINT ( 'NONE',  ( 18.65267415280877117, -0.4843198157805662651, -217.0419311198673711 ) ) ;
#10973 = VERTEX_POINT ( 'NONE', #9655 ) ;
#10974 = ORIENTED_EDGE ( 'NONE', *, *, #2230, .T. ) ;
#10975 = CARTESIAN_POINT ( 'NONE',  ( 14.69879291197755222, 10.86005690695417236, -216.7815908316746913 ) ) ;
#10976 = CARTESIAN_POINT ( 'NONE',  ( -18.67270963783218463, 15.11229250701181925, -218.9067109956068578 ) ) ;
#10977 = CARTESIAN_POINT ( 'NONE',  ( 13.85822045549773129, -1.469587484828172919, -226.8778453516271156 ) ) ;
#10978 = CARTESIAN_POINT ( 'NONE',  ( -3.176860551132370425, -19.01962362838126452, -231.5826211182368297 ) ) ;
#10979 = CARTESIAN_POINT ( 'NONE',  ( 0.000000000000000000, 0.000000000000000000, -30.00000000000000000 ) ) ;
#10980 = ORIENTED_EDGE ( 'NONE', *, *, #16436, .T. ) ;
#10981 = CARTESIAN_POINT ( 'NONE',  ( 15.12287735332712835, 21.03907941686458116, -231.7894952627153202 ) ) ;
#10982 = CARTESIAN_POINT ( 'NONE',  ( -32.05942529185317369, -1.254016050025921425, -226.3193970476597485 ) ) ;
#10983 = CARTESIAN_POINT ( 'NONE',  ( -18.05576253097465766, 2.935622250037499104, -232.1557308718028594 ) ) ;
#10984 = AXIS2_PLACEMENT_3D ( 'NONE', #8788, #15650, #19445 ) ;
#10985 = AXIS2_PLACEMENT_3D ( 'NONE', #21410, #6108, #825 ) ;
#10986 = CARTESIAN_POINT ( 'NONE',  ( 11.14834367153813233, -21.42845646353120870, -216.4520112529555718 ) ) ;
#10987 =( LENGTH_UNIT ( ) NAMED_UNIT ( * ) SI_UNIT ( .MILLI., .METRE. ) );
#10988 = CARTESIAN_POINT ( 'NONE',  ( 0.9046320824004248085, 13.39785254849979701, -226.4815711199935890 ) ) ;
#10989 = CARTESIAN_POINT ( 'NONE',  ( -11.27928845652762213, 14.86256579634383002, -216.2427993537644966 ) ) ;
#10990 = ORIENTED_EDGE ( 'NONE', *, *, #2596, .T. ) ;
#10991 = CARTESIAN_POINT ( 'NONE',  ( -9.749377714296398878, 10.28442384816749922, -229.3722863967025205 ) ) ;
#10992 = CARTESIAN_POINT ( 'NONE',  ( -23.85568197540453994, -15.41036827548725618, -219.8503866864575969 ) ) ;
#10993 = FACE_BOUND ( 'NONE', #10407, .T. ) ;
#10994 = PLANE ( 'NONE',  #11649 ) ;
#10995 = CARTESIAN_POINT ( 'NONE',  ( -14.73016414256368911, 22.23431809695627237, -217.1425123644553707 ) ) ;
#10996 = CARTESIAN_POINT ( 'NONE',  ( 7.896007729111394369, -13.22437314876957437, -221.6501328817743683 ) ) ;
#10997 =( NAMED_UNIT ( * ) PLANE_ANGLE_UNIT ( ) SI_UNIT ( $, .RADIAN. ) );
#10998 = CARTESIAN_POINT ( 'NONE',  ( -15.48255455842386219, 10.01793346089237069, -233.1197357361336913 ) ) ;
#10999 = ADVANCED_BREP_SHAPE_REPRESENTATION ( '', ( #22038, #6677 ), #1652 ) ;
#11000 = EDGE_CURVE ( 'NONE', #3205, #19675, #20094, .T. ) ;
#11001 = CARTESIAN_POINT ( 'NONE',  ( -11.36937006530106586, 5.486019310970209339, -224.0742584078730033 ) ) ;
#11002 = CARTESIAN_POINT ( 'NONE',  ( -1.946052076048385482, 22.23149728939677061, -232.8927760318659068 ) ) ;
#11003 = DIRECTION ( 'NONE',  ( 0.000000000000000000, 0.000000000000000000, 1.000000000000000000 ) ) ;
#11004 = CARTESIAN_POINT ( 'NONE',  ( 19.10353041285295816, 2.510539514498965730, -232.1135168369976896 ) ) ;
#11005 = CARTESIAN_POINT ( 'NONE',  ( -10.44804907229818980, -15.26164834479392240, -220.3887109030195859 ) ) ;
#11006 = AXIS2_PLACEMENT_3D ( 'NONE', #4328, #2974, #18411 ) ;
#11007 = ORIENTED_EDGE ( 'NONE', *, *, #14912, .F. ) ;
#11008 = CARTESIAN_POINT ( 'NONE',  ( 5.803912621764987456, 13.01725692290267844, -221.8367675400179166 ) ) ;
#11009 = CARTESIAN_POINT ( 'NONE',  ( -11.86888352782322897, 15.29489941890347282, -218.1379771575364259 ) ) ;
#11010 = CARTESIAN_POINT ( 'NONE',  ( -8.463283775975803280, 12.69606588598396613, -228.6351674091961286 ) ) ;
#11011 = CARTESIAN_POINT ( 'NONE',  ( -15.91852731338648752, -4.625608912867816613, -229.2691880628015895 ) ) ;
#11012 = DIRECTION ( 'NONE',  ( 1.000000000000000000, 0.000000000000000000, 0.000000000000000000 ) ) ;
#11013 = ORIENTED_EDGE ( 'NONE', *, *, #16421, .F. ) ;
#11014 = CARTESIAN_POINT ( 'NONE',  ( 15.70515172005171323, -0.7403987186381333352, -226.4590404369862995 ) ) ;
#11015 = CARTESIAN_POINT ( 'NONE',  ( 6.726326701167932853, -14.50135447204537087, -224.8733857281379755 ) ) ;
#11016 = CARTESIAN_POINT ( 'NONE',  ( 22.02796522526679723, 16.41909032291435366, -220.1590600991317217 ) ) ;
#11017 = CARTESIAN_POINT ( 'NONE',  ( 5.331555957413248059, 27.50712867803999728, -219.0801070358024276 ) ) ;
#11018 = AXIS2_PLACEMENT_3D ( 'NONE', #8877, #15741, #19095 ) ;
#11019 = CARTESIAN_POINT ( 'NONE',  ( -22.18165477997343871, 9.502253276305026475, -218.0070055737419636 ) ) ;
#11020 = CARTESIAN_POINT ( 'NONE',  ( 19.66580438618080251, 15.18147523775131624, -233.5153994334876586 ) ) ;
#11021 = CARTESIAN_POINT ( 'NONE',  ( 10.57926812561479757, 10.00910231482511215, -225.8341706491384286 ) ) ;
#11022 = DIRECTION ( 'NONE',  ( 0.000000000000000000, 0.000000000000000000, 1.000000000000000000 ) ) ;
#11023 = CARTESIAN_POINT ( 'NONE',  ( -11.49803752765619258, -8.459563989871591971, -222.4296168992866853 ) ) ;
#11024 = CARTESIAN_POINT ( 'NONE',  ( 8.510712203779903007, -27.79691582975998898, -230.5316902582456180 ) ) ;
#11025 = CARTESIAN_POINT ( 'NONE',  ( 12.50000000000000355, 0.000000000000000000, -70.00000000000000000 ) ) ;
#11026 = EDGE_CURVE ( 'NONE', #11155, #2762, #9695, .T. ) ;
#11027 = FACE_OUTER_BOUND ( 'NONE', #623, .T. ) ;
#11028 = CARTESIAN_POINT ( 'NONE',  ( -16.58369694688956741, 24.75758513462668375, -230.3405478298966784 ) ) ;
#11029 = CARTESIAN_POINT ( 'NONE',  ( 11.86238739854314872, -1.469869507039519130, -223.6725020993723660 ) ) ;
#11030 = CARTESIAN_POINT ( 'NONE',  ( 24.59129902578158067, -8.191391589517788674, -218.4338547727923299 ) ) ;
#11031 = CARTESIAN_POINT ( 'NONE',  ( 21.38922145650625239, 17.10616209967719215, -217.8354246241890451 ) ) ;
#11032 = CARTESIAN_POINT ( 'NONE',  ( 10.64724148863252395, 12.28344647332184181, -223.6549461381946173 ) ) ;
#11033 = VERTEX_POINT ( 'NONE', #18319 ) ;
#11034 = CARTESIAN_POINT ( 'NONE',  ( 12.30978816035033496, -6.276705103789536722, -231.2162571060900405 ) ) ;
#11035 = CARTESIAN_POINT ( 'NONE',  ( 14.19800769603076240, 4.587407146151301518, -224.2928935459285071 ) ) ;
#11036 = EDGE_CURVE ( 'NONE', #16801, #13087, #10099, .T. ) ;
#11037 = CARTESIAN_POINT ( 'NONE',  ( 1.920320557106582893, 25.99317453242502296, -234.5637964893073217 ) ) ;
#11038 = CARTESIAN_POINT ( 'NONE',  ( -8.005900519654911562, 11.01772743098285545, -228.7074549843708269 ) ) ;
#11039 = CARTESIAN_POINT ( 'NONE',  ( -21.94776718874828347, -0.4748437386657700099, -216.1214812709574176 ) ) ;
#11040 = CARTESIAN_POINT ( 'NONE',  ( -18.47334320050258327, 24.79293862780133040, -226.9986786077537317 ) ) ;
#11041 = CARTESIAN_POINT ( 'NONE',  ( 14.50000000000000178, -3.976862775871337963, 93.00000000000001421 ) ) ;
#11042 = CARTESIAN_POINT ( 'NONE',  ( 24.59129902578158067, -8.191391589517788674, -218.4338547727923299 ) ) ;
#11043 = CARTESIAN_POINT ( 'NONE',  ( -6.388048297418547961, 21.92257289597608150, -233.3290245341164848 ) ) ;
#11044 = CARTESIAN_POINT ( 'NONE',  ( 22.17049319811867036, 0.5483778423327810847, -216.5715983009590673 ) ) ;
#11045 = CARTESIAN_POINT ( 'NONE',  ( -12.31207293045244988, 6.732038552366256923, -221.0952066824360713 ) ) ;
#11046 = CARTESIAN_POINT ( 'NONE',  ( 19.19288224840068935, 10.13059690604263174, -232.1906135022504998 ) ) ;
#11047 = CARTESIAN_POINT ( 'NONE',  ( -28.12632608809566293, -1.403418003803144742, -218.5233027210585988 ) ) ;
#11048 = EDGE_LOOP ( 'NONE', ( #7492, #8102, #5624, #7079 ) ) ;
#11049 = CARTESIAN_POINT ( 'NONE',  ( 2.914696262605396715, 19.49933023975583879, -231.6035545612375017 ) ) ;
#11050 = CARTESIAN_POINT ( 'NONE',  ( -14.78079095050690661, -5.416970230978240153, -229.7193632018645246 ) ) ;
#11051 = CARTESIAN_POINT ( 'NONE',  ( 4.301648988406530094, 13.23079486486395240, -223.2766268961034655 ) ) ;
#11052 = CARTESIAN_POINT ( 'NONE',  ( -7.242471263717580321, -12.67345288765796774, -222.7008556220510229 ) ) ;
#11053 = CARTESIAN_POINT ( 'NONE',  ( -23.00000000000000000, 0.000000000000000000, 75.00000000000000000 ) ) ;
#11054 = CARTESIAN_POINT ( 'NONE',  ( -13.51406939156936104, 10.04301168678160749, -230.1761202643687056 ) ) ;
#11055 = CARTESIAN_POINT ( 'NONE',  ( -29.43130594997593974, -3.977420319584657360, -224.3854249914923571 ) ) ;
#11056 = CARTESIAN_POINT ( 'NONE',  ( 3.528957931946373971, 27.43889307663531696, -223.4805233499528185 ) ) ;
#11057 = CARTESIAN_POINT ( 'NONE',  ( -14.69827142695382527, 14.49176359921644597, -217.9600391472806109 ) ) ;
#11058 = CARTESIAN_POINT ( 'NONE',  ( -24.77996431573922820, 10.49354383977773786, -234.1655613096203581 ) ) ;
#11059 = CARTESIAN_POINT ( 'NONE',  ( -9.870642741937645681, -28.68889699630894441, -223.8025096038410879 ) ) ;
#11060 = CARTESIAN_POINT ( 'NONE',  ( 25.12984891811676036, 19.96069634721137476, -226.7154725927711070 ) ) ;
#11061 = FACE_OUTER_BOUND ( 'NONE', #4170, .T. ) ;
#11062 = CARTESIAN_POINT ( 'NONE',  ( -18.68851093906118521, -8.564152624513159395, -215.1804141040323941 ) ) ;
#11063 = CARTESIAN_POINT ( 'NONE',  ( -1.772400894765090662, 19.49811434610897010, -217.8797837662441168 ) ) ;
#11064 = CARTESIAN_POINT ( 'NONE',  ( -22.10934047915413814, 0.9940043559354462266, -218.9999999999999716 ) ) ;
#11065 = CARTESIAN_POINT ( 'NONE',  ( -5.854583994961135573, 13.10358817970001866, -222.4168379437668648 ) ) ;
#11066 = ADVANCED_FACE ( 'NONE', ( #11895 ), #10211, .F. ) ;
#11067 = CARTESIAN_POINT ( 'NONE',  ( 19.20222574149634909, 21.83532798770326266, -218.6913543321078919 ) ) ;
#11068 = ORIENTED_EDGE ( 'NONE', *, *, #9658, .F. ) ;
#11069 = CARTESIAN_POINT ( 'NONE',  ( -3.159549884399295294, -15.02780241139942952, -220.2520066652115531 ) ) ;
#11070 = CARTESIAN_POINT ( 'NONE',  ( 3.619268272960482591, -21.10655420957111517, -217.8630709410095108 ) ) ;
#11071 = ADVANCED_FACE ( 'NONE', ( #6377 ), #9136, .T. ) ;
#11072 = CARTESIAN_POINT ( 'NONE',  ( 1.526556658859590748E-13, -21.00000000000006395, -75.00000000000000000 ) ) ;
#11073 = CARTESIAN_POINT ( 'NONE',  ( 25.69300549816939494, 5.947472783069708946, -230.6131061331718115 ) ) ;
#11074 = CARTESIAN_POINT ( 'NONE',  ( 20.80196158924851701, -7.261721507697286526, -217.3074963141844194 ) ) ;
#11075 = ADVANCED_FACE ( 'NONE', ( #13249 ), #16516, .T. ) ;
#11076 = CARTESIAN_POINT ( 'NONE',  ( -9.078153229956912540, -10.71731945587431056, -228.5228069477245469 ) ) ;
#11077 = CARTESIAN_POINT ( 'NONE',  ( -6.512931564893298386, -17.32529878264574563, -216.7284160531958719 ) ) ;
#11078 = CARTESIAN_POINT ( 'NONE',  ( 8.179023008129211902, 20.84698146175953681, -218.6376653143925921 ) ) ;
#11079 = LINE ( 'NONE', #7488, #15215 ) ;
#11080 = CARTESIAN_POINT ( 'NONE',  ( 22.24262848503957812, 2.205713500382371794, -232.7243927205662430 ) ) ;
#11081 = CARTESIAN_POINT ( 'NONE',  ( -6.282398543089500187, 12.01615879894893801, -228.5121145169883903 ) ) ;
#11082 = CARTESIAN_POINT ( 'NONE',  ( 3.614175329767659761, 21.98488100320606264, -219.0898850257099753 ) ) ;
#11083 = CARTESIAN_POINT ( 'NONE',  ( 15.97952439233267263, -1.339455371059026456, -231.0376074705642395 ) ) ;
#11084 = ORIENTED_EDGE ( 'NONE', *, *, #10571, .F. ) ;
#11085 = CARTESIAN_POINT ( 'NONE',  ( 11.01659168199870287, 19.17922986229587323, -233.3715978632214387 ) ) ;
#11086 = CARTESIAN_POINT ( 'NONE',  ( -17.30580402557236752, 11.30149179219993982, -230.8639894634705172 ) ) ;
#11087 = CARTESIAN_POINT ( 'NONE',  ( 29.08100487150598212, 12.14819438347179670, -226.9621620069135020 ) ) ;
#11088 = CARTESIAN_POINT ( 'NONE',  ( -1.380908993000753648, -20.21092959135559752, -218.0995018783601438 ) ) ;
#11089 = DIRECTION ( 'NONE',  ( 0.000000000000000000, 0.000000000000000000, -1.000000000000000000 ) ) ;
#11090 = ORIENTED_EDGE ( 'NONE', *, *, #16135, .F. ) ;
#11091 = CARTESIAN_POINT ( 'NONE',  ( 17.97843143658897347, 22.12221935793617078, -220.9346589834416079 ) ) ;
#11092 = CARTESIAN_POINT ( 'NONE',  ( 20.16749130626988773, -19.72590806003585229, -223.0880382675181579 ) ) ;
#11093 = CARTESIAN_POINT ( 'NONE',  ( -20.45797657813638182, 1.164962349958370336, -217.1306074022350572 ) ) ;
#11094 = VECTOR ( 'NONE', #12557, 1000.000000000000000 ) ;
#11095 = CARTESIAN_POINT ( 'NONE',  ( -10.42804209284631156, -14.08702332024887305, -217.7386024361820489 ) ) ;
#11096 = CARTESIAN_POINT ( 'NONE',  ( 4.389496648589924277, 14.47660514356954131, -220.6151178996808540 ) ) ;
#11097 = CARTESIAN_POINT ( 'NONE',  ( -0.8357710952364670876, 15.48480697989137234, -216.9118565312697910 ) ) ;
#11098 = EDGE_LOOP ( 'NONE', ( #20681, #16985, #18711, #3859, #4740, #3491 ) ) ;
#11099 = CARTESIAN_POINT ( 'NONE',  ( -21.02719846458807851, 18.12262440796364871, -218.0220709499931502 ) ) ;
#11100 = CARTESIAN_POINT ( 'NONE',  ( 26.82025090637478115, -4.850230565203020205, -219.1860060474940042 ) ) ;
#11101 = DIRECTION ( 'NONE',  ( 1.000000000000000000, 0.000000000000000000, -0.000000000000000000 ) ) ;
#11102 = CARTESIAN_POINT ( 'NONE',  ( -21.17702599587410717, 8.978242263026027459, -4.451669607260716255 ) ) ;
#11103 = CARTESIAN_POINT ( 'NONE',  ( -6.201839134465864767, 11.37481922992157379, -223.7040893475979146 ) ) ;
#11104 = CARTESIAN_POINT ( 'NONE',  ( 2.018545692720245643, -30.97649562252411215, -224.4812544443210811 ) ) ;
#11105 = CARTESIAN_POINT ( 'NONE',  ( 15.50779141722566656, -5.694711448414747856, -219.6385356284298211 ) ) ;
#11106 = CARTESIAN_POINT ( 'NONE',  ( -13.83274569775339202, 16.20364235096346661, -234.0851861771356539 ) ) ;
#11107 = CARTESIAN_POINT ( 'NONE',  ( -13.34869474643618581, 6.516017165032126357, -231.2228057326931321 ) ) ;
#11108 = CARTESIAN_POINT ( 'NONE',  ( -1.973648319964989462, 15.33498294326524203, -220.9958390492969329 ) ) ;
#11109 = VECTOR ( 'NONE', #5710, 1000.000000000000000 ) ;
#11110 = CYLINDRICAL_SURFACE ( 'NONE', #16278, 4.100000000000000533 ) ;
#11111 = CARTESIAN_POINT ( 'NONE',  ( 21.43345597994050777, 2.294722475943265838, -232.7243927205661294 ) ) ;
#11112 = CARTESIAN_POINT ( 'NONE',  ( -14.02781974392415165, -24.18658813864446344, -225.1634145543362706 ) ) ;
#11113 = ORIENTED_EDGE ( 'NONE', *, *, #11545, .F. ) ;
#11114 = CARTESIAN_POINT ( 'NONE',  ( 17.24952650401854370, 25.19767938110938843, -224.5319471861414797 ) ) ;
#11115 = CARTESIAN_POINT ( 'NONE',  ( -8.900302563431933933, 20.17395648083808268, -216.9116515890487733 ) ) ;
#11116 = CARTESIAN_POINT ( 'NONE',  ( -9.115411286166651195, 13.66191091052436235, -230.3338332872444312 ) ) ;
#11117 = CARTESIAN_POINT ( 'NONE',  ( -29.37537067777813604, -4.151788015186005154, -225.5750753894876368 ) ) ;
#11118 = DIRECTION ( 'NONE',  ( 0.000000000000000000, -1.000000000000000000, 0.000000000000000000 ) ) ;
#11119 = VERTEX_POINT ( 'NONE', #15168 ) ;
#11120 = CARTESIAN_POINT ( 'NONE',  ( 17.47660375112063491, 0.1533180678384444551, -220.6249646429494931 ) ) ;
#11121 = CARTESIAN_POINT ( 'NONE',  ( -4.075588186332946172, -27.83231707117609588, -229.7735430035053810 ) ) ;
#11122 = CARTESIAN_POINT ( 'NONE',  ( 27.04607490430786854, 4.607450003618843049, -220.3758934308003461 ) ) ;
#11123 = CARTESIAN_POINT ( 'NONE',  ( -3.205260335674071648, 17.52234722004434531, -232.9754319808710363 ) ) ;
#11124 = CARTESIAN_POINT ( 'NONE',  ( 15.02522163627726037, -2.279509738242128769, -223.0471089487919585 ) ) ;
#11125 = CARTESIAN_POINT ( 'NONE',  ( -28.00010259152825398, 3.831607968041374157, -225.8381323513402208 ) ) ;
#11126 = CARTESIAN_POINT ( 'NONE',  ( 7.116434306140963173, 9.967665124511082553, -224.4990387090310833 ) ) ;
#11127 = CARTESIAN_POINT ( 'NONE',  ( 22.02796522526679723, 16.41909032291435366, -220.1590600991317217 ) ) ;
#11128 = CARTESIAN_POINT ( 'NONE',  ( 25.50000000000000000, 0.5000000000000000000, 0.000000000000000000 ) ) ;
#11129 = CARTESIAN_POINT ( 'NONE',  ( -12.00435701841128022, -1.798699874815819166, -227.7674894005143074 ) ) ;
#11130 = CARTESIAN_POINT ( 'NONE',  ( -21.28605893225895684, -20.43870967537180050, -221.0356759888913700 ) ) ;
#11131 = CARTESIAN_POINT ( 'NONE',  ( 6.260999666360449467, -13.19315344885661645, -220.2890618333529744 ) ) ;
#11132 = LINE ( 'NONE', #2890, #4492 ) ;
#11133 = DIRECTION ( 'NONE',  ( -1.000000000000000000, 0.000000000000000000, 0.000000000000000000 ) ) ;
#11134 = CARTESIAN_POINT ( 'NONE',  ( -2.043230952238195286, 23.63069326910348877, -232.6835180461029040 ) ) ;
#11135 = CARTESIAN_POINT ( 'NONE',  ( 29.01190720243894461, 0.5135883731763817295, -231.9442528450179566 ) ) ;
#11136 = CARTESIAN_POINT ( 'NONE',  ( 13.28406271702445274, -5.237238614233280742, -225.2640488721434622 ) ) ;
#11137 = CARTESIAN_POINT ( 'NONE',  ( -18.74633356284308761, 11.17209001323738704, -217.5809474206552068 ) ) ;
#11138 = CARTESIAN_POINT ( 'NONE',  ( 16.64575860537911112, 25.12688477742292648, -227.5050599151411745 ) ) ;
#11139 = CARTESIAN_POINT ( 'NONE',  ( 14.12692363916921146, 20.59586666873830296, -230.0804552526094540 ) ) ;
#11140 = ORIENTED_EDGE ( 'NONE', *, *, #3893, .F. ) ;
#11141 = CARTESIAN_POINT ( 'NONE',  ( 4.746237488610151267, -29.30821474977460639, -222.1257927337785247 ) ) ;
#11142 = CARTESIAN_POINT ( 'NONE',  ( -21.63401512838757768, 0.000000000000000000, -77.51594804401857175 ) ) ;
#11143 = CARTESIAN_POINT ( 'NONE',  ( -12.15711705271618470, 28.08001788883979799, -220.3431297925021681 ) ) ;
#11144 = CARTESIAN_POINT ( 'NONE',  ( -13.24620988741752825, 28.78239319002125285, -225.3527830703614256 ) ) ;
#11145 = CARTESIAN_POINT ( 'NONE',  ( -14.84457943406284208, -4.054717634150219574, -219.4128920803699430 ) ) ;
#11146 = CARTESIAN_POINT ( 'NONE',  ( -7.429838964355703901, 14.87322129099639234, -232.2632863647814077 ) ) ;
#11147 = CARTESIAN_POINT ( 'NONE',  ( 8.999942255032404859, -11.40691176929436068, 93.00000000000000000 ) ) ;
#11148 = EDGE_CURVE ( 'NONE', #5788, #3240, #2992, .T. ) ;
#11149 = CARTESIAN_POINT ( 'NONE',  ( 20.80196158924851701, -7.261721507697286526, -217.3074963141844194 ) ) ;
#11150 = CARTESIAN_POINT ( 'NONE',  ( -5.854583994961135573, 13.10358817970001866, -222.4168379437668648 ) ) ;
#11151 = CARTESIAN_POINT ( 'NONE',  ( 20.64287812348744566, 0.2024751443801864337, -216.7518974727033481 ) ) ;
#11152 = CARTESIAN_POINT ( 'NONE',  ( -15.82069055112642353, 8.315535108674763976, -217.2800172218543935 ) ) ;
#11153 = CARTESIAN_POINT ( 'NONE',  ( 26.29894631880581812, 12.29609390142961090, -226.3100047295820332 ) ) ;
#11154 = CARTESIAN_POINT ( 'NONE',  ( 15.63557944520553988, 0.5893374091412190152, -227.9430452042592208 ) ) ;
#11155 = VERTEX_POINT ( 'NONE', #16963 ) ;
#11156 = CARTESIAN_POINT ( 'NONE',  ( 5.066530254613678785, 15.76189963344335254, -222.1234037505291781 ) ) ;
#11157 = CARTESIAN_POINT ( 'NONE',  ( -18.75993824683981970, -9.028840681436806292, -217.1556094966459227 ) ) ;
#11158 = CARTESIAN_POINT ( 'NONE',  ( 26.24002132888527328, 11.62331517472360964, -222.5300873157218859 ) ) ;
#11159 = CARTESIAN_POINT ( 'NONE',  ( 0.2060740257213805326, -13.46849591350090947, -221.0879548523055860 ) ) ;
#11160 = CARTESIAN_POINT ( 'NONE',  ( 0.000000000000000000, 23.00000000000000000, 75.00000000000000000 ) ) ;
#11161 = CARTESIAN_POINT ( 'NONE',  ( -21.66803296057637951, 19.04503900041684616, -222.6603677762044526 ) ) ;
#11162 = CARTESIAN_POINT ( 'NONE',  ( 10.05661706967825353, -14.25456047934742365, -218.9909083857680230 ) ) ;
#11163 = CARTESIAN_POINT ( 'NONE',  ( 15.56183105618911355, 23.93598532278018354, -223.2746693648072664 ) ) ;
#11164 = CARTESIAN_POINT ( 'NONE',  ( -14.24491355791863612, 5.286533920242113105, -221.7104936369346433 ) ) ;
#11165 = CARTESIAN_POINT ( 'NONE',  ( -29.15345109632842124, 14.07532767497844262, -225.0972140442887621 ) ) ;
#11166 = CARTESIAN_POINT ( 'NONE',  ( -16.33212578464095799, -13.18764990320557118, -218.7248530738716283 ) ) ;
#11167 = CARTESIAN_POINT ( 'NONE',  ( 16.84354851290083133, 10.42424693870724361, -215.2582953371023109 ) ) ;
#11168 = DIRECTION ( 'NONE',  ( -1.000000000000000000, 0.000000000000000000, -0.000000000000000000 ) ) ;
#11169 = CARTESIAN_POINT ( 'NONE',  ( -21.92622494339052608, -22.07770017127804962, -220.0303431275545165 ) ) ;
#11170 = CARTESIAN_POINT ( 'NONE',  ( 3.846342036506673612, 16.55327908958690131, -231.1358846258000597 ) ) ;
#11171 = CARTESIAN_POINT ( 'NONE',  ( 26.59731715018858011, 13.56210517473685329, -229.5787264587298466 ) ) ;
#11172 = CARTESIAN_POINT ( 'NONE',  ( -13.06839468023815165, 25.32320678245788059, -229.0099538679170053 ) ) ;
#11173 = CARTESIAN_POINT ( 'NONE',  ( 3.672031556878595282, 11.54613252248376831, -227.4694100414545801 ) ) ;
#11174 = EDGE_CURVE ( 'NONE', #14013, #13305, #16660, .T. ) ;
#11175 = ORIENTED_EDGE ( 'NONE', *, *, #19320, .T. ) ;
#11176 = CARTESIAN_POINT ( 'NONE',  ( -5.579930056231209967, -28.86398153493815144, -221.8494056429758814 ) ) ;
#11177 = EDGE_LOOP ( 'NONE', ( #17966, #13696 ) ) ;
#11178 = CARTESIAN_POINT ( 'NONE',  ( 6.869068212838696397, -24.78254998730118430, -231.2855974421026986 ) ) ;
#11179 = CARTESIAN_POINT ( 'NONE',  ( 24.57222455393806015, 12.08236629421828212, -229.7319216558644541 ) ) ;
#11180 = CARTESIAN_POINT ( 'NONE',  ( 11.43609017326686050, -13.06727081285745307, -217.8903327850316316 ) ) ;
#11181 = CARTESIAN_POINT ( 'NONE',  ( 14.01369322398082851, -0.3099216430074364093, -221.6784101578248283 ) ) ;
#11182 = CARTESIAN_POINT ( 'NONE',  ( -17.42499862437977853, -18.98713029041037004, -232.7811807006768845 ) ) ;
#11183 = CARTESIAN_POINT ( 'NONE',  ( 15.56183105618911355, 23.93598532278018354, -223.2746693648072664 ) ) ;
#11184 =( LENGTH_UNIT ( ) NAMED_UNIT ( * ) SI_UNIT ( .MILLI., .METRE. ) );
#11185 = CARTESIAN_POINT ( 'NONE',  ( 18.39384604806649648, 2.566915855367216004, -231.7421336352533103 ) ) ;
#11186 = CARTESIAN_POINT ( 'NONE',  ( 0.4042326456706432647, 15.50845657815858303, -219.2680337625893401 ) ) ;
#11187 = CARTESIAN_POINT ( 'NONE',  ( 7.508136856874425114, 24.19512352541684663, -230.0608033085341617 ) ) ;
#11188 = CARTESIAN_POINT ( 'NONE',  ( 22.24262848504226042, 2.205713500382400216, -232.7243927205662999 ) ) ;
#11189 = ORIENTED_EDGE ( 'NONE', *, *, #8488, .F. ) ;
#11190 = CARTESIAN_POINT ( 'NONE',  ( 10.70175380652492336, 7.370128018021000038, -224.3479584370086286 ) ) ;
#11191 = CARTESIAN_POINT ( 'NONE',  ( -14.46024998630872282, 14.54669730493860946, -231.4156670963686508 ) ) ;
#11192 = CARTESIAN_POINT ( 'NONE',  ( -27.32994399549947673, 3.379920396491164603, -227.9326384921875217 ) ) ;
#11193 = EDGE_CURVE ( 'NONE', #12695, #12719, #9876, .T. ) ;
#11194 = CARTESIAN_POINT ( 'NONE',  ( 1.268102448827562068, -18.18084990330622830, -231.0699201170278911 ) ) ;
#11195 = DIRECTION ( 'NONE',  ( -1.000000000000000000, 0.000000000000000000, 0.000000000000000000 ) ) ;
#11196 = DIRECTION ( 'NONE',  ( -1.000000000000000000, 0.000000000000000000, 0.000000000000000000 ) ) ;
#11197 = CARTESIAN_POINT ( 'NONE',  ( 4.354034006296288339, 14.09944204372416188, -221.2519525881239417 ) ) ;
#11198 = CARTESIAN_POINT ( 'NONE',  ( 17.09791731880535437, -14.50769433911838568, -231.1780219065761059 ) ) ;
#11199 = DIRECTION ( 'NONE',  ( 1.000000000000000000, 0.000000000000000000, 6.123233995736766036E-17 ) ) ;
#11200 = CARTESIAN_POINT ( 'NONE',  ( -8.514447835183077018, -10.26590951297754195, -225.5321622820681569 ) ) ;
#11201 = CARTESIAN_POINT ( 'NONE',  ( -3.501680520304516264, 14.31538576447642264, -219.8967178229432307 ) ) ;
#11202 = VECTOR ( 'NONE', #9022, 1000.000000000000000 ) ;
#11203 = CARTESIAN_POINT ( 'NONE',  ( -4.378220565073127624, 31.53459173284372952, -222.0564199190954753 ) ) ;
#11204 = ORIENTED_EDGE ( 'NONE', *, *, #13812, .F. ) ;
#11205 = CARTESIAN_POINT ( 'NONE',  ( -9.540790481621398200, 9.981116473660406996, -228.6478862620407995 ) ) ;
#11206 = CARTESIAN_POINT ( 'NONE',  ( -21.27082149447729620, -6.316573346028001801, -216.2864220516500779 ) ) ;
#11207 = CARTESIAN_POINT ( 'NONE',  ( 29.82766783012230505, -1.714217446056379934, -229.3564438616236316 ) ) ;
#11208 = CARTESIAN_POINT ( 'NONE',  ( -23.00000000000007105, 0.3345464022992510333, -10.00000000000000000 ) ) ;
#11209 = CARTESIAN_POINT ( 'NONE',  ( -13.83274569775339202, 16.20364235096346661, -234.0851861771356539 ) ) ;
#11210 = CARTESIAN_POINT ( 'NONE',  ( -22.35094797335686678, -23.29487558099128108, -223.4832390375085538 ) ) ;
#11211 = DIRECTION ( 'NONE',  ( -1.000000000000000000, 0.000000000000000000, 0.000000000000000000 ) ) ;
#11212 = CARTESIAN_POINT ( 'NONE',  ( -22.17339560624464312, 16.26550580028390769, -232.0582861498566274 ) ) ;
#11213 = CIRCLE ( 'NONE', #1505, 21.00000000000008171 ) ;
#11214 = CARTESIAN_POINT ( 'NONE',  ( -12.12559971566433958, 1.856299769312002912, -227.8748781050665286 ) ) ;
#11215 = CARTESIAN_POINT ( 'NONE',  ( 1.313727069624702981, 17.80710275190598324, -219.4197901500037062 ) ) ;
#11216 = DIRECTION ( 'NONE',  ( 0.000000000000000000, 0.000000000000000000, -1.000000000000000000 ) ) ;
#11217 = CARTESIAN_POINT ( 'NONE',  ( -21.07387565400155438, 1.107905485989369554, -215.0000000023499069 ) ) ;
#11218 = CARTESIAN_POINT ( 'NONE',  ( -16.14140970932308505, -18.57031478189210816, -230.2506069696216287 ) ) ;
#11219 = ORIENTED_EDGE ( 'NONE', *, *, #1722, .T. ) ;
#11220 = CARTESIAN_POINT ( 'NONE',  ( 10.49811526528768368, 13.26166588535847701, -217.9009921269571919 ) ) ;
#11221 = CARTESIAN_POINT ( 'NONE',  ( 1.773237071419721422, 13.09828209437875302, -220.6531024550077404 ) ) ;
#11222 = CARTESIAN_POINT ( 'NONE',  ( -13.40354389326479456, 23.35336998323175450, -219.8517474526506987 ) ) ;
#11223 = CIRCLE ( 'NONE', #11948, 21.99162546567091070 ) ;
#11224 = CARTESIAN_POINT ( 'NONE',  ( -25.45695634607983848, -10.72451519803311015, -228.5848280742264933 ) ) ;
#11225 = VERTEX_POINT ( 'NONE', #8192 ) ;
#11226 = CARTESIAN_POINT ( 'NONE',  ( 17.28149325064817887, -1.074788064772476792, -229.5315781944399305 ) ) ;
#11227 = CARTESIAN_POINT ( 'NONE',  ( -3.159549884399295294, -15.02780241139942952, -220.2520066652115531 ) ) ;
#11228 = CARTESIAN_POINT ( 'NONE',  ( 15.61962121506769385, 4.525360868525488911, -229.0684696061408090 ) ) ;
#11229 = CARTESIAN_POINT ( 'NONE',  ( 4.543450689403089271, 15.91052110650461771, -218.9437823786444426 ) ) ;
#11230 = CARTESIAN_POINT ( 'NONE',  ( 14.81724556832271311, -2.803809140094828400, -226.0847343491304855 ) ) ;
#11231 = CARTESIAN_POINT ( 'NONE',  ( -15.10760069511485604, 3.026516874529453283, -224.5685390982118861 ) ) ;
#11232 = CARTESIAN_POINT ( 'NONE',  ( 11.84598249547323690, 10.36127485500543699, -218.5481300776139904 ) ) ;
#11233 = TOROIDAL_SURFACE ( 'NONE', #11586, 24.63401512838747820, 3.000000000000000888 ) ;
#11234 = DIRECTION ( 'NONE',  ( 1.000000000000000000, 0.000000000000000000, 0.000000000000000000 ) ) ;
#11235 = CARTESIAN_POINT ( 'NONE',  ( 21.39553407250273054, 8.453402029343234148, -217.9531594780983141 ) ) ;
#11236 = DIRECTION ( 'NONE',  ( 0.000000000000000000, 0.000000000000000000, -1.000000000000000000 ) ) ;
#11237 = CARTESIAN_POINT ( 'NONE',  ( 27.51601410384567359, -3.359424968747257711, -222.6356212526655725 ) ) ;
#11238 = CARTESIAN_POINT ( 'NONE',  ( -18.11268275035277853, -3.459088653808292335, -218.4233329573673359 ) ) ;
#11239 = CARTESIAN_POINT ( 'NONE',  ( -23.00000000000006750, -1.237926774615798086E-16, -10.00000000000000000 ) ) ;
#11240 = LINE ( 'NONE', #16423, #18435 ) ;
#11241 = CARTESIAN_POINT ( 'NONE',  ( -9.439286754415764591, 28.32957437491962338, -228.7842975624562598 ) ) ;
#11242 = CARTESIAN_POINT ( 'NONE',  ( 29.53814377227115884, -10.02285884041311270, -220.1614914916521286 ) ) ;
#11243 = CARTESIAN_POINT ( 'NONE',  ( 24.96294718070021901, -13.86220829677249178, -229.4442241490162075 ) ) ;
#11244 = CARTESIAN_POINT ( 'NONE',  ( -16.27882490622757672, 1.520697279646460398, -219.2607721384596289 ) ) ;
#11245 = CARTESIAN_POINT ( 'NONE',  ( 8.592982993077152187, 10.20906991731218838, -226.0923132092261483 ) ) ;
#11246 = CARTESIAN_POINT ( 'NONE',  ( 21.07144422417032104, 18.33581350331571969, -223.6711752364813890 ) ) ;
#11247 = EDGE_CURVE ( 'NONE', #862, #10234, #1208, .T. ) ;
#11248 = ORIENTED_EDGE ( 'NONE', *, *, #16821, .T. ) ;
#11249 = CARTESIAN_POINT ( 'NONE',  ( 0.3267584840439746174, -16.39795729406718650, -220.1296710765888065 ) ) ;
#11250 = CARTESIAN_POINT ( 'NONE',  ( 0.000000000000000000, 0.000000000000000000, -65.00000000000000000 ) ) ;
#11251 = AXIS2_PLACEMENT_3D ( 'NONE', #15075, #19067, #288 ) ;
#11252 = CARTESIAN_POINT ( 'NONE',  ( 3.982203626615636427, 14.63895582687697150, -217.4952312584269123 ) ) ;
#11253 = CARTESIAN_POINT ( 'NONE',  ( -7.403072389817287657, 18.92851032520892929, -215.2068968469505137 ) ) ;
#11254 = CARTESIAN_POINT ( 'NONE',  ( 23.56599333006272445, -4.960096179470117050, -217.5996013647105372 ) ) ;
#11255 = CARTESIAN_POINT ( 'NONE',  ( -4.104500432947460808, 15.73223271406093460, -218.0734292856946297 ) ) ;
#11256 = CARTESIAN_POINT ( 'NONE',  ( 1.526556658859590243E-13, -21.00000000000000000, -75.00000000000000000 ) ) ;
#11257 =( NAMED_UNIT ( * ) SI_UNIT ( $, .STERADIAN. ) SOLID_ANGLE_UNIT ( ) );
#11258 = CARTESIAN_POINT ( 'NONE',  ( -1.884624261322229266, 13.00421381464247084, -226.7648460381863345 ) ) ;
#11259 = CARTESIAN_POINT ( 'NONE',  ( -16.23590288079963173, 0.2625226423351309513, -226.8300841971807813 ) ) ;
#11260 = CARTESIAN_POINT ( 'NONE',  ( -12.90983082593748676, 14.84936372681532823, -233.8009687022269532 ) ) ;
#11261 = CARTESIAN_POINT ( 'NONE',  ( 12.85408565574548412, 7.821283853063205171, -223.1248833997948111 ) ) ;
#11262 = AXIS2_PLACEMENT_3D ( 'NONE', #6775, #6662, #11949 ) ;
#11263 = CARTESIAN_POINT ( 'NONE',  ( 4.555016420009541989, 17.65848956729471197, -229.5875910199184204 ) ) ;
#11264 = VECTOR ( 'NONE', #5251, 1000.000000000000000 ) ;
#11265 = DIRECTION ( 'NONE',  ( -0.000000000000000000, -0.000000000000000000, -1.000000000000000000 ) ) ;
#11266 = CARTESIAN_POINT ( 'NONE',  ( 8.250760074138732136, 14.96691001493985951, -221.7548416114337613 ) ) ;
#11267 = CARTESIAN_POINT ( 'NONE',  ( -8.878187501988019648, -11.23476449186280846, -221.0271673637577123 ) ) ;
#11268 = CARTESIAN_POINT ( 'NONE',  ( 23.04897566969193079, 17.95862962700741861, -223.6438515760422661 ) ) ;
#11269 = CARTESIAN_POINT ( 'NONE',  ( -4.538939863750555581, -15.27574540357637112, -231.4384328720293524 ) ) ;
#11270 = CARTESIAN_POINT ( 'NONE',  ( 18.76166303929373314, 2.999999999999994227, -224.8778586954795742 ) ) ;
#11271 = CARTESIAN_POINT ( 'NONE',  ( -16.07193224038526580, 12.24477688577882439, -232.1409653212175499 ) ) ;
#11272 = ADVANCED_FACE ( 'NONE', ( #21790, #21899 ), #1093, .F. ) ;
#11273 = CARTESIAN_POINT ( 'NONE',  ( 24.68599888815047194, -16.20242508705913309, -228.6174911781957633 ) ) ;
#11274 = CARTESIAN_POINT ( 'NONE',  ( 3.388180927852674884, 15.71154068801650538, -224.9339660840813053 ) ) ;
#11275 = CARTESIAN_POINT ( 'NONE',  ( -13.51406939156936104, 10.04301168678160749, -230.1761202643687056 ) ) ;
#11276 = CARTESIAN_POINT ( 'NONE',  ( -15.35982698007958724, 5.508237851081846159, -233.6994028941782631 ) ) ;
#11277 = CARTESIAN_POINT ( 'NONE',  ( -22.93937586921525806, -8.311597057603599126, -230.3633560851501159 ) ) ;
#11278 = CARTESIAN_POINT ( 'NONE',  ( 13.32754126089433377, 12.31312334927721963, -234.6033665822900218 ) ) ;
#11279 = VECTOR ( 'NONE', #1690, 1000.000000000000000 ) ;
#11280 = DIRECTION ( 'NONE',  ( 1.000000000000000000, 4.408728476930457445E-15, 0.000000000000000000 ) ) ;
#11281 = CARTESIAN_POINT ( 'NONE',  ( -7.264683844434491000, -10.24731347617596100, -229.2886802738593985 ) ) ;
#11282 = CARTESIAN_POINT ( 'NONE',  ( 10.31623634631035991, 26.83927646318382898, -220.2315638557092541 ) ) ;
#11283 = CARTESIAN_POINT ( 'NONE',  ( 17.29648694364601980, 10.20782262162153842, -233.8400727604031317 ) ) ;
#11284 = CARTESIAN_POINT ( 'NONE',  ( -10.07004052286948337, 22.64471483900350179, -217.4645417110143626 ) ) ;
#11285 = CARTESIAN_POINT ( 'NONE',  ( 4.966801760238292118, 27.41406605988239420, -216.4490579899774900 ) ) ;
#11286 = CARTESIAN_POINT ( 'NONE',  ( 0.1655890855189643129, -14.86936674525315993, -225.9040401458518943 ) ) ;
#11287 = VERTEX_POINT ( 'NONE', #21676 ) ;
#11288 = CARTESIAN_POINT ( 'NONE',  ( 5.920190106170357680, -27.41802839654005197, -221.0732524667164114 ) ) ;
#11289 = CARTESIAN_POINT ( 'NONE',  ( 16.00819137755116373, 4.595691552992191120, -229.5669508871464757 ) ) ;
#11290 = CARTESIAN_POINT ( 'NONE',  ( 13.96958060839473958, -9.488587112651741151, -218.7731372952745232 ) ) ;
#11291 = CARTESIAN_POINT ( 'NONE',  ( -28.87859926594958537, -0.8320174534291842061, -222.6356913548140142 ) ) ;
#11292 = CARTESIAN_POINT ( 'NONE',  ( -8.491902988188710921, -10.37035003683405066, -223.9502466269643435 ) ) ;
#11293 = ADVANCED_FACE ( 'NONE', ( #22010 ), #9991, .F. ) ;
#11294 = CARTESIAN_POINT ( 'NONE',  ( 13.41709597927210496, 19.57823531746157997, -218.2666972400567147 ) ) ;
#11295 = SURFACE_STYLE_USAGE ( .BOTH. , #13207 ) ;
#11296 = CARTESIAN_POINT ( 'NONE',  ( 19.79854089336508594, 4.557290221971136646, -217.3342919181881143 ) ) ;
#11297 = CIRCLE ( 'NONE', #21696, 21.00000000000008527 ) ;
#11298 = CARTESIAN_POINT ( 'NONE',  ( -0.1571923090946999446, 19.34188126963334398, -216.6893131123363787 ) ) ;
#11299 = CARTESIAN_POINT ( 'NONE',  ( -0.6272116608575281083, 20.18031380156121202, -219.3960054794027030 ) ) ;
#11300 = CARTESIAN_POINT ( 'NONE',  ( 12.77158894069672357, -20.43488010613652150, -235.1868042311012914 ) ) ;
#11301 = CARTESIAN_POINT ( 'NONE',  ( 11.43247012502872728, 12.44034019618676190, -231.9336559008378629 ) ) ;
#11302 = CARTESIAN_POINT ( 'NONE',  ( -18.59263364681495290, 22.28600439725833482, -224.9897462721271779 ) ) ;
#11303 = CARTESIAN_POINT ( 'NONE',  ( -19.50431861204945605, -0.7624880359591150736, -219.4666829195064395 ) ) ;
#11304 = CARTESIAN_POINT ( 'NONE',  ( 1.167080303844580058, -21.82675117811238152, -232.1335090276773485 ) ) ;
#11305 = DIRECTION ( 'NONE',  ( 1.000000000000000000, -0.000000000000000000, -0.000000000000000000 ) ) ;
#11306 = CARTESIAN_POINT ( 'NONE',  ( -20.99999999999999645, 0.000000000000000000, -60.00000000000001421 ) ) ;
#11307 = ADVANCED_FACE ( 'NONE', ( #6269, #16626, #19988 ), #1428, .T. ) ;
#11308 = CARTESIAN_POINT ( 'NONE',  ( 26.48990917286906921, 12.16675355942207659, -225.0153622588060216 ) ) ;
#11309 = CARTESIAN_POINT ( 'NONE',  ( 14.07866085257239419, -11.11077054092157645, -229.4139412770749971 ) ) ;
#11310 = DIRECTION ( 'NONE',  ( -1.000000000000000000, -1.224646799147352961E-16, 0.000000000000000000 ) ) ;
#11311 = CARTESIAN_POINT ( 'NONE',  ( -11.40116373163465369, -15.95513543764466213, -216.7841692646331353 ) ) ;
#11312 = DIRECTION ( 'NONE',  ( 1.000000000000000000, 0.000000000000000000, 0.000000000000000000 ) ) ;
#11313 = CARTESIAN_POINT ( 'NONE',  ( -3.368164009525018265, 19.03203264544105622, -233.5986411977714567 ) ) ;
#11314 = CARTESIAN_POINT ( 'NONE',  ( 3.744112528862662881, 31.76296354843916703, -227.8872370379487506 ) ) ;
#11315 = ORIENTED_EDGE ( 'NONE', *, *, #22048, .T. ) ;
#11316 = CARTESIAN_POINT ( 'NONE',  ( -18.70100282803782576, 16.58357028540773115, -216.4425743468854080 ) ) ;
#11317 = CARTESIAN_POINT ( 'NONE',  ( -28.09913862414779473, -9.456046895945956265, -221.0065986266286870 ) ) ;
#11318 = PRESENTATION_LAYER_ASSIGNMENT (  '', '', ( #21017 ) ) ;
#11319 = CARTESIAN_POINT ( 'NONE',  ( 27.12528000378512871, -1.050705938820645224, -232.4139529590446784 ) ) ;
#11320 = DIRECTION ( 'NONE',  ( -0.000000000000000000, -1.000000000000000000, 0.000000000000000000 ) ) ;
#11321 = CARTESIAN_POINT ( 'NONE',  ( -8.172572110426221670, 16.86653848210977813, -233.4220330256369493 ) ) ;
#11322 = CARTESIAN_POINT ( 'NONE',  ( -6.616223485457675579, -9.589312190179589024, -225.7195100648197581 ) ) ;
#11323 = CARTESIAN_POINT ( 'NONE',  ( 19.06212547406409641, -9.287000003594721775, -232.7453815625877667 ) ) ;
#11324 = CARTESIAN_POINT ( 'NONE',  ( -22.11084984981285118, 10.96048252433489623, -216.6117774006995376 ) ) ;
#11325 = CARTESIAN_POINT ( 'NONE',  ( -20.05025075566126702, 1.207204931470905018, -215.1628017022767949 ) ) ;
#11326 = CARTESIAN_POINT ( 'NONE',  ( 5.585286719045844173, 27.51657303716567426, -222.4190945945824751 ) ) ;
#11327 = CYLINDRICAL_SURFACE ( 'NONE', #19488, 23.00000000000000000 ) ;
#11328 = CARTESIAN_POINT ( 'NONE',  ( -14.99655511003079233, 2.316638599135941945, -232.4215266639120046 ) ) ;
#11329 = CARTESIAN_POINT ( 'NONE',  ( -7.469054245001129466, -18.21857363335801594, -219.2823717272210047 ) ) ;
#11330 = EDGE_LOOP ( 'NONE', ( #7421, #18893, #17633, #15312 ) ) ;
#11331 = CARTESIAN_POINT ( 'NONE',  ( -10.29720673141181209, 11.14783905173092649, -222.8560683878917530 ) ) ;
#11332 = CARTESIAN_POINT ( 'NONE',  ( 7.772443558932104146, 25.24620711463332157, -231.7813173736589931 ) ) ;
#11333 = CARTESIAN_POINT ( 'NONE',  ( -5.762781846020777365, 12.94769902409342777, -223.1319556069387886 ) ) ;
#11334 = ORIENTED_EDGE ( 'NONE', *, *, #16505, .T. ) ;
#11335 = CARTESIAN_POINT ( 'NONE',  ( 22.46263922039936745, -3.404486942579552089, -216.1438077301478415 ) ) ;
#11336 = CARTESIAN_POINT ( 'NONE',  ( 0.000000000000000000, 0.000000000000000000, -75.00000000000000000 ) ) ;
#11337 = AXIS2_PLACEMENT_3D ( 'NONE', #15980, #2128, #2018 ) ;
#11338 = ORIENTED_EDGE ( 'NONE', *, *, #18602, .F. ) ;
#11339 = CARTESIAN_POINT ( 'NONE',  ( -22.17339560624464312, 16.26550580028390769, -232.0582861498566274 ) ) ;
#11340 = CARTESIAN_POINT ( 'NONE',  ( -12.42003616114091358, -24.71691410793946986, -217.8239624370676779 ) ) ;
#11341 = DIRECTION ( 'NONE',  ( -0.000000000000000000, 0.000000000000000000, -1.000000000000000000 ) ) ;
#11342 = CARTESIAN_POINT ( 'NONE',  ( 11.57669841200422134, 10.63052136557218574, -228.9489978335593889 ) ) ;
#11343 = CARTESIAN_POINT ( 'NONE',  ( 25.50000000000000000, 3.600000000000000533, -2.700000000000000622 ) ) ;
#11344 = CARTESIAN_POINT ( 'NONE',  ( 14.95834318372430083, -1.617016552789838801, -229.6306532055809271 ) ) ;
#11345 = CARTESIAN_POINT ( 'NONE',  ( 24.78222556642275620, 17.97262539535998371, -226.6641400693514470 ) ) ;
#11346 =( LENGTH_UNIT ( ) NAMED_UNIT ( * ) SI_UNIT ( .MILLI., .METRE. ) );
#11347 = CARTESIAN_POINT ( 'NONE',  ( 15.42019186727181257, 1.458536399438582043, -222.3758756028272785 ) ) ;
#11348 = ADVANCED_FACE ( 'NONE', ( #20315 ), #4910, .F. ) ;
#11349 = CARTESIAN_POINT ( 'NONE',  ( 18.23324537670537993, 23.47692953258263771, -224.8333321331434433 ) ) ;
#11350 = DIRECTION ( 'NONE',  ( 0.000000000000000000, 0.000000000000000000, -1.000000000000000000 ) ) ;
#11351 = CARTESIAN_POINT ( 'NONE',  ( 15.35804315687698107, -7.528275283329426415, -228.0874909612831232 ) ) ;
#11352 = CARTESIAN_POINT ( 'NONE',  ( -25.42089018817326007, -6.263968923056941307, -218.6542964065910439 ) ) ;
#11353 = EDGE_CURVE ( 'NONE', #20454, #9399, #17746, .T. ) ;
#11354 = CARTESIAN_POINT ( 'NONE',  ( 24.99999999999999645, 1.360023205165816762E-13, 0.000000000000000000 ) ) ;
#11355 = CARTESIAN_POINT ( 'NONE',  ( -23.00000000000000000, 0.000000000000000000, -24.99999999999999645 ) ) ;
#11356 = CARTESIAN_POINT ( 'NONE',  ( -7.312583518931054627, 16.22063427959223958, -217.3454962955413521 ) ) ;
#11357 = CARTESIAN_POINT ( 'NONE',  ( 12.24504971509987072, -1.481354005294047926, -221.9045230856115438 ) ) ;
#11358 = CARTESIAN_POINT ( 'NONE',  ( 29.12543877365354916, -1.475122899492763873, -224.0746120762670444 ) ) ;
#11359 = CARTESIAN_POINT ( 'NONE',  ( -27.92885697401080591, 6.962042978589167319, -220.9552227796709190 ) ) ;
#11360 = CARTESIAN_POINT ( 'NONE',  ( 13.30790133003807441, 0.6370684082013071681, -222.3495379725305270 ) ) ;
#11361 = CARTESIAN_POINT ( 'NONE',  ( 19.59567110982616001, 18.11097967140601028, -228.7314497914969706 ) ) ;
#11362 = EDGE_LOOP ( 'NONE', ( #12567, #19213, #2686, #11764, #5263, #19302 ) ) ;
#11363 = CARTESIAN_POINT ( 'NONE',  ( 5.902215564816073012, -11.20991439657816358, -226.4118943921501170 ) ) ;
#11364 = CARTESIAN_POINT ( 'NONE',  ( 13.96913104090061886, 4.808762379633894746, 93.00000000000002842 ) ) ;
#11365 = CARTESIAN_POINT ( 'NONE',  ( -26.98548179121306845, 3.096138561569834913, -233.8324893795610251 ) ) ;
#11366 = CARTESIAN_POINT ( 'NONE',  ( 11.00045714400293306, 20.20239058357963913, -215.1666500215986275 ) ) ;
#11367 = CARTESIAN_POINT ( 'NONE',  ( 0.9169988354999972779, 20.59043933275470550, -235.2854195559275752 ) ) ;
#11368 = CARTESIAN_POINT ( 'NONE',  ( 26.82025090637478115, -4.850230565203020205, -219.1860060474940042 ) ) ;
#11369 = CARTESIAN_POINT ( 'NONE',  ( -2.772442535524381579, 13.75675912271027457, -228.9770533867650215 ) ) ;
#11370 = LINE ( 'NONE', #17907, #7261 ) ;
#11371 = AXIS2_PLACEMENT_3D ( 'NONE', #8926, #8816, #15792 ) ;
#11372 = MECHANICAL_DESIGN_GEOMETRIC_PRESENTATION_REPRESENTATION (  '', ( #21055 ), #12454 ) ;
#11373 = CARTESIAN_POINT ( 'NONE',  ( -6.415689407129693045, 29.32186846096819011, -228.3852515614991887 ) ) ;
#11374 = CARTESIAN_POINT ( 'NONE',  ( -14.58670098223046629, 7.239570004716886942, -229.3284954533748135 ) ) ;
#11375 = CARTESIAN_POINT ( 'NONE',  ( -17.65835845419170624, 22.55329142274348442, -231.2673511165784532 ) ) ;
#11376 = CARTESIAN_POINT ( 'NONE',  ( 23.04897566969193079, 17.95862962700741861, -223.6438515760422661 ) ) ;
#11377 = CARTESIAN_POINT ( 'NONE',  ( 8.829458998963966465, 22.90677303676718779, -219.2026791561175685 ) ) ;
#11378 = CARTESIAN_POINT ( 'NONE',  ( 1.232595164407830946E-29, -17.50000000000007105, -55.00000000000000000 ) ) ;
#11379 = CARTESIAN_POINT ( 'NONE',  ( 12.94599882983645145, 15.82237817288049442, -219.3332542656393116 ) ) ;
#11380 = CARTESIAN_POINT ( 'NONE',  ( -16.75313578746775889, -14.38352658620038937, -216.6304878158699978 ) ) ;
#11381 = CARTESIAN_POINT ( 'NONE',  ( 15.61962121506769385, 4.525360868525488911, -229.0684696061408090 ) ) ;
#11382 = CARTESIAN_POINT ( 'NONE',  ( -6.532222827695542300, -22.16123078269809099, -233.6760793125601481 ) ) ;
#11383 = CARTESIAN_POINT ( 'NONE',  ( 0.000000000000000000, 23.00000000000000000, 75.00000000000000000 ) ) ;
#11384 = CARTESIAN_POINT ( 'NONE',  ( -9.627017372966443887, 15.60690227900018279, -218.8878023709062859 ) ) ;
#11385 =( NAMED_UNIT ( * ) SI_UNIT ( $, .STERADIAN. ) SOLID_ANGLE_UNIT ( ) );
#11386 = CARTESIAN_POINT ( 'NONE',  ( 16.43596176044053081, -17.06621466254232544, -232.8418678805942648 ) ) ;
#11387 = CARTESIAN_POINT ( 'NONE',  ( 19.13999328532042910, 9.776920959053244431, -216.1190985676915375 ) ) ;
#11388 = CARTESIAN_POINT ( 'NONE',  ( -15.51982305277792307, 19.76957551617798359, -231.4018974401358832 ) ) ;
#11389 = CARTESIAN_POINT ( 'NONE',  ( -23.68377094563794572, 13.02263794644603578, -215.9752901280847652 ) ) ;
#11390 = CARTESIAN_POINT ( 'NONE',  ( -14.27403737459813193, -10.90264666745762057, -220.2309642783388597 ) ) ;
#11391 = CARTESIAN_POINT ( 'NONE',  ( -18.93763370444446181, -0.7340653299870684156, -219.7345063954518594 ) ) ;
#11392 = DIRECTION ( 'NONE',  ( -1.000000000000000000, 0.000000000000000000, 0.000000000000000000 ) ) ;
#11393 = CARTESIAN_POINT ( 'NONE',  ( -18.15502857810558268, -5.877683472035677426, -234.3930847616834683 ) ) ;
#11394 = CARTESIAN_POINT ( 'NONE',  ( -4.855966894080006035, 26.75753167227873064, -230.1547293463117114 ) ) ;
#11395 = CARTESIAN_POINT ( 'NONE',  ( -19.11923763334766946, 1.257783214997954202, -219.7591028439344711 ) ) ;
#11396 = CARTESIAN_POINT ( 'NONE',  ( -9.679547659771646551, 14.60131434979866505, -230.4338124916943968 ) ) ;
#11397 = CARTESIAN_POINT ( 'NONE',  ( 3.889974896201825239, 13.98719620150063214, -218.1465764473210527 ) ) ;
#11398 = EDGE_LOOP ( 'NONE', ( #10124, #17672, #19566, #9320 ) ) ;
#11399 = CARTESIAN_POINT ( 'NONE',  ( -4.075588186332946172, -27.83231707117609588, -229.7735430035053810 ) ) ;
#11400 = ORIENTED_EDGE ( 'NONE', *, *, #17132, .F. ) ;
#11401 = CARTESIAN_POINT ( 'NONE',  ( -1.434166139689934338, -16.90223958437590213, -219.9603817157532433 ) ) ;
#11402 = CARTESIAN_POINT ( 'NONE',  ( -31.84745724608465522, 5.474219582435353004, -224.7210333253351564 ) ) ;
#11403 = CARTESIAN_POINT ( 'NONE',  ( 13.04434844185555420, -10.19049307777131297, -230.8679447648462713 ) ) ;
#11404 = CARTESIAN_POINT ( 'NONE',  ( 23.45680152528306550, 2.072154465955917235, -232.7243927205664704 ) ) ;
#11405 = CARTESIAN_POINT ( 'NONE',  ( -6.870552667427666904, -18.85419487977974029, -216.2130481585807047 ) ) ;
#11406 = CARTESIAN_POINT ( 'NONE',  ( 4.044213993247089967, 16.45246633354041421, -227.9255899743332918 ) ) ;
#11407 = LINE ( 'NONE', #18276, #920 ) ;
#11408 = CARTESIAN_POINT ( 'NONE',  ( -15.05930145804884290, 24.78193219970826533, -223.0510781988847953 ) ) ;
#11409 = CARTESIAN_POINT ( 'NONE',  ( 12.10245006109274080, 26.02147364279441888, -220.6079829738538649 ) ) ;
#11410 = CARTESIAN_POINT ( 'NONE',  ( 9.575488824002899690, 13.89846378187365694, -220.1158735840035945 ) ) ;
#11411 = CARTESIAN_POINT ( 'NONE',  ( 11.58852274881379962, -8.803378160360782800, -231.6724139265004965 ) ) ;
#11412 = CARTESIAN_POINT ( 'NONE',  ( 8.554868430186942874, 10.42313681336814568, -223.0114508542762621 ) ) ;
#11413 = CARTESIAN_POINT ( 'NONE',  ( -13.91323058514953637, 8.006348396443080162, -225.5064972756604220 ) ) ;
#11414 = CARTESIAN_POINT ( 'NONE',  ( -3.515149843921121509, -20.22121776728782550, -231.9652171757311123 ) ) ;
#11415 = CARTESIAN_POINT ( 'NONE',  ( 0.000000000000000000, 0.000000000000000000, -103.0000000000000000 ) ) ;
#11416 = DIRECTION ( 'NONE',  ( 0.000000000000000000, 0.000000000000000000, 1.000000000000000000 ) ) ;
#11417 = ADVANCED_FACE ( 'NONE', ( #191 ), #12330, .F. ) ;
#11418 = CARTESIAN_POINT ( 'NONE',  ( 15.87442104186276381, 8.674488492264579520, -230.9702037640878416 ) ) ;
#11419 = CARTESIAN_POINT ( 'NONE',  ( 19.11859169356911536, -17.02155004481861411, -230.1485466288596911 ) ) ;
#11420 = DIRECTION ( 'NONE',  ( 1.000000000000000000, 0.000000000000000000, -0.000000000000000000 ) ) ;
#11421 = CARTESIAN_POINT ( 'NONE',  ( -3.734153817218577309, -19.72686645808614614, -233.9207428641194610 ) ) ;
#11422 = CONTEXT_DEPENDENT_SHAPE_REPRESENTATION ( #20631, #21972 ) ;
#11423 = CARTESIAN_POINT ( 'NONE',  ( -2.808235066048971440, 30.42019778760651150, -222.6481917607299295 ) ) ;
#11424 = CARTESIAN_POINT ( 'NONE',  ( -0.6224962293416278492, 14.12372964796689701, -218.2103911528446645 ) ) ;
#11425 = EDGE_LOOP ( 'NONE', ( #19427, #18134 ) ) ;
#11426 = CARTESIAN_POINT ( 'NONE',  ( -3.082945806077231676, 30.69897765966285874, -224.2387254578930822 ) ) ;
#11427 = CARTESIAN_POINT ( 'NONE',  ( 21.75737151495774313, -2.205713500382427750, -233.2756072794337285 ) ) ;
#11428 = CARTESIAN_POINT ( 'NONE',  ( -24.99350385409967856, -0.6578573476328165581, 9.983793171540982669 ) ) ;
#11429 = CARTESIAN_POINT ( 'NONE',  ( -17.50000000000000355, 2.143131898507868643E-15, -65.00000000000000000 ) ) ;
#11430 = CARTESIAN_POINT ( 'NONE',  ( 4.603870848087811218, 30.13529352683433515, -225.9623629403671430 ) ) ;
#11431 = CARTESIAN_POINT ( 'NONE',  ( -1.821616882984092411, -20.20372127477041246, -234.2708619787750308 ) ) ;
#11432 = CARTESIAN_POINT ( 'NONE',  ( 24.96294718070021901, -13.86220829677249178, -229.4442241490162075 ) ) ;
#11433 = CARTESIAN_POINT ( 'NONE',  ( -4.104500432947460808, 15.73223271406093460, -218.0734292856946297 ) ) ;
#11434 = CARTESIAN_POINT ( 'NONE',  ( 21.43345597994050777, 2.294722475943265838, -232.7243927205661294 ) ) ;
#11435 = CARTESIAN_POINT ( 'NONE',  ( 1.719513778997906694, 15.52930330544231730, -222.3959083836286368 ) ) ;
#11436 = CARTESIAN_POINT ( 'NONE',  ( 0.000000000000000000, 0.000000000000000000, 75.00000000000000000 ) ) ;
#11437 = CARTESIAN_POINT ( 'NONE',  ( 19.79854089336508594, 4.557290221971136646, -217.3342919181881143 ) ) ;
#11438 = CARTESIAN_POINT ( 'NONE',  ( -15.48718561803335625, -8.207282836869444154, -229.3046138068065147 ) ) ;
#11439 = ORIENTED_EDGE ( 'NONE', *, *, #3565, .T. ) ;
#11440 = CARTESIAN_POINT ( 'NONE',  ( -18.74633356284308761, 11.17209001323738704, -217.5809474206552068 ) ) ;
#11441 = CARTESIAN_POINT ( 'NONE',  ( 3.160467108836292116, 14.95099014189016629, -228.9242958482614370 ) ) ;
#11442 = CARTESIAN_POINT ( 'NONE',  ( -1.806671251568986669, 13.52068930966770388, -228.3567401718105430 ) ) ;
#11443 = AXIS2_PLACEMENT_3D ( 'NONE', #8295, #8525, #11783 ) ;
#11444 = CARTESIAN_POINT ( 'NONE',  ( -24.05661684749028240, -8.720095227435134433, -219.0096885115910084 ) ) ;
#11445 = CARTESIAN_POINT ( 'NONE',  ( 13.80743592543072396, -3.637675435010108906E-12, -228.0000000000000568 ) ) ;
#11446 = ORIENTED_EDGE ( 'NONE', *, *, #13649, .T. ) ;
#11447 = CARTESIAN_POINT ( 'NONE',  ( -12.90983082593748676, 14.84936372681532823, -233.8009687022269532 ) ) ;
#11448 = CARTESIAN_POINT ( 'NONE',  ( -3.786803964513834941, -14.74062382431161566, -229.2965385003435586 ) ) ;
#11449 = CARTESIAN_POINT ( 'NONE',  ( 15.35712710306588846, 1.253371448057428283, -227.7275853420972567 ) ) ;
#11450 = CARTESIAN_POINT ( 'NONE',  ( 9.333020543840051531, 16.91085096921651143, -217.7308990335875762 ) ) ;
#11451 = DIRECTION ( 'NONE',  ( 0.000000000000000000, 0.000000000000000000, -1.000000000000000000 ) ) ;
#11452 = UNCERTAINTY_MEASURE_WITH_UNIT (LENGTH_MEASURE( 1.000000000000000082E-05 ), #17010, 'distance_accuracy_value', 'NONE');
#11453 = CARTESIAN_POINT ( 'NONE',  ( -19.98042543492610079, 23.51949599776966693, -226.6701036947414138 ) ) ;
#11454 = CARTESIAN_POINT ( 'NONE',  ( 25.60482246989237609, 8.614967517510873307, -219.3103232513597618 ) ) ;
#11455 = CARTESIAN_POINT ( 'NONE',  ( -23.18379035723104664, 9.355751749453526500, -3.546302055531801223 ) ) ;
#11456 = CARTESIAN_POINT ( 'NONE',  ( 18.83090365933348664, -2.940867245730338642, -224.3956276138626720 ) ) ;
#11457 = DIRECTION ( 'NONE',  ( 0.000000000000000000, 0.000000000000000000, 1.000000000000000000 ) ) ;
#11458 = CARTESIAN_POINT ( 'NONE',  ( -23.67094103897667523, 1.103242709927489740, -215.1660654633311935 ) ) ;
#11460 = ADVANCED_FACE ( 'NONE', ( #10133 ), #15322, .F. ) ;
#11459 = CARTESIAN_POINT ( 'NONE',  ( -24.92024473536680773, -13.74570206812420103, -220.1598944320903115 ) ) ;
#11461 = CARTESIAN_POINT ( 'NONE',  ( 0.000000000000000000, 23.00000000000006040, 69.99999999999998579 ) ) ;
#11462 = CARTESIAN_POINT ( 'NONE',  ( -13.17897211815351000, 23.48099580033777301, -217.3415693533541173 ) ) ;
#11463 = CARTESIAN_POINT ( 'NONE',  ( 11.42868579270797369, -5.440147491673143598, -220.7688621915004603 ) ) ;
#11464 = CARTESIAN_POINT ( 'NONE',  ( 29.17814965709308694, -1.309718763918959139, -225.2029557489520926 ) ) ;
#11465 = CARTESIAN_POINT ( 'NONE',  ( -22.38347148959098121, 12.58966534755613687, -218.4978713241202399 ) ) ;
#11466 = CARTESIAN_POINT ( 'NONE',  ( -21.48978835671764287, 1.062155088816892468, -219.0000000007146355 ) ) ;
#11467 = CARTESIAN_POINT ( 'NONE',  ( 15.70200226922815290, 22.14006925444000018, -227.8255507828836244 ) ) ;
#11468 = EDGE_LOOP ( 'NONE', ( #9290, #15701, #19332, #2285 ) ) ;
#11469 = CARTESIAN_POINT ( 'NONE',  ( -0.6911605129178206575, -19.14003671809244267, -232.0914249810984131 ) ) ;
#11470 = CARTESIAN_POINT ( 'NONE',  ( -2.025093002184608082, 14.49031849020018647, 93.00000000000000000 ) ) ;
#11471 = CARTESIAN_POINT ( 'NONE',  ( -12.61443312487471324, 8.399394471292156439, -217.5740162615319093 ) ) ;
#11472 = CARTESIAN_POINT ( 'NONE',  ( 12.99334571784053338, 27.47142594410712846, -219.5003755906066658 ) ) ;
#11473 = CARTESIAN_POINT ( 'NONE',  ( 3.672031556878595282, 11.54613252248376831, -227.4694100414545801 ) ) ;
#11474 = CARTESIAN_POINT ( 'NONE',  ( 23.44453178257692727, -8.594063734448958769, -231.6993511358095361 ) ) ;
#11475 = EDGE_CURVE ( 'NONE', #16180, #16938, #21691, .T. ) ;
#11476 = CARTESIAN_POINT ( 'NONE',  ( -3.501680520304516264, 14.31538576447642264, -219.8967178229432307 ) ) ;
#11477 = CARTESIAN_POINT ( 'NONE',  ( -13.93333636822611155, 3.327141996558931947, -221.4468162587888287 ) ) ;
#11478 = CARTESIAN_POINT ( 'NONE',  ( 18.65058977333779211, 24.40868228550881014, -219.3406275662563303 ) ) ;
#11479 = CARTESIAN_POINT ( 'NONE',  ( -15.10760069511485604, 3.026516874529453283, -224.5685390982118861 ) ) ;
#11480 = CARTESIAN_POINT ( 'NONE',  ( -19.25929423112888017, 9.818144317380269825, -216.1837936240308409 ) ) ;
#11481 = CARTESIAN_POINT ( 'NONE',  ( 28.51464931495100785, 5.422321182929326966, -223.8116416110474347 ) ) ;
#11482 = CARTESIAN_POINT ( 'NONE',  ( 7.487569386194327770, 15.49107591903592862, -229.0624668269501001 ) ) ;
#11483 = DIRECTION ( 'NONE',  ( 0.000000000000000000, 0.000000000000000000, 1.000000000000000000 ) ) ;
#11484 = DIRECTION ( 'NONE',  ( -0.000000000000000000, -1.000000000000000000, -0.000000000000000000 ) ) ;
#11485 = CARTESIAN_POINT ( 'NONE',  ( 14.72046356508972309, 21.23077830076469041, -229.4562045376679578 ) ) ;
#11486 = CARTESIAN_POINT ( 'NONE',  ( -13.21314811618155716, -9.038438575223175064, -230.6430079410957603 ) ) ;
#11487 = CARTESIAN_POINT ( 'NONE',  ( 14.63113973005795643, 4.926264598692385199, -222.4866305912601945 ) ) ;
#11488 = CARTESIAN_POINT ( 'NONE',  ( -3.482364789216947809, -21.46714584935086023, -216.0234696677019883 ) ) ;
#11489 = DIRECTION ( 'NONE',  ( 0.000000000000000000, 0.000000000000000000, 1.000000000000000000 ) ) ;
#11490 = CARTESIAN_POINT ( 'NONE',  ( -12.67219131930435694, 19.52425521811199971, -218.0046184995277372 ) ) ;
#11491 = CARTESIAN_POINT ( 'NONE',  ( 24.99999999999999645, 1.372269673157290277E-13, -10.00000000000000000 ) ) ;
#11492 = CARTESIAN_POINT ( 'NONE',  ( 10.73531068932428667, -10.59494929936097307, -229.0901643129046192 ) ) ;
#11493 = CARTESIAN_POINT ( 'NONE',  ( 12.63974878616558328, 15.03448928898568759, -231.7036488814491406 ) ) ;
#11494 = CARTESIAN_POINT ( 'NONE',  ( -10.70754874174748039, 23.84972878377777405, -230.7991598016655246 ) ) ;
#11495 = CARTESIAN_POINT ( 'NONE',  ( -11.89542918462869103, -0.2773029175206048191, -224.4556830488584467 ) ) ;
#11496 = CARTESIAN_POINT ( 'NONE',  ( -22.37826137345437871, -13.90312800710061047, -229.3506127454622572 ) ) ;
#11497 = CARTESIAN_POINT ( 'NONE',  ( 27.08260752785270853, 4.114838227474355570, -232.2882281786467331 ) ) ;
#11498 = CARTESIAN_POINT ( 'NONE',  ( 0.000000000000000000, 0.000000000000000000, -65.00000000000000000 ) ) ;
#11499 = CARTESIAN_POINT ( 'NONE',  ( -14.27185570462694919, -0.4134134650712557035, -229.5903738612280449 ) ) ;
#11500 = CARTESIAN_POINT ( 'NONE',  ( 10.70175380652492336, 7.370128018021000038, -224.3479584370086286 ) ) ;
#11501 = CARTESIAN_POINT ( 'NONE',  ( 14.33191776452776622, 5.147404080619256916, -219.0172570056664938 ) ) ;
#11502 = CARTESIAN_POINT ( 'NONE',  ( 2.471991688031208945, 13.88348721647344419, -230.6707754746932437 ) ) ;
#11503 = ADVANCED_BREP_SHAPE_REPRESENTATION ( '', ( #21655, #6677 ), #8455 ) ;
#11504 = CARTESIAN_POINT ( 'NONE',  ( 17.10545320562996352, 22.53742678899184781, -232.4605876935045785 ) ) ;
#11505 = CARTESIAN_POINT ( 'NONE',  ( 1.672997396509183110, -28.78979777605457713, -223.2908548649682814 ) ) ;
#11506 = ORIENTED_EDGE ( 'NONE', *, *, #12730, .F. ) ;
#11507 = CARTESIAN_POINT ( 'NONE',  ( 7.074707374710634156, -26.72731565888815553, -229.5909540767539738 ) ) ;
#11508 = CARTESIAN_POINT ( 'NONE',  ( -9.503027668167838726, 6.959046566381404730, -225.7241663910276941 ) ) ;
#11509 = CARTESIAN_POINT ( 'NONE',  ( 13.28406271702445274, -5.237238614233280742, -225.2640488721434622 ) ) ;
#11510 = CARTESIAN_POINT ( 'NONE',  ( -25.42089018817326007, -6.263968923056941307, -218.6542964065910439 ) ) ;
#11511 = CARTESIAN_POINT ( 'NONE',  ( -12.44777057840899559, -8.577008958641105352, -229.4809580173677830 ) ) ;
#11512 = CARTESIAN_POINT ( 'NONE',  ( 8.645835506124264214, 12.38899589144949687, -223.4673650485651990 ) ) ;
#11513 = CARTESIAN_POINT ( 'NONE',  ( -14.01966324001334385, 10.60695606488527964, -217.6333332521996340 ) ) ;
#11514 = CARTESIAN_POINT ( 'NONE',  ( 19.13999328532042910, 9.776920959053244431, -216.1190985676915375 ) ) ;
#11515 = CARTESIAN_POINT ( 'NONE',  ( 2.008896548638861024, 20.64812324442097591, -233.5818019448501843 ) ) ;
#11516 = CARTESIAN_POINT ( 'NONE',  ( 12.55473222622303986, 11.30320364856893001, -218.8964119182764989 ) ) ;
#11517 = CARTESIAN_POINT ( 'NONE',  ( 10.88154471369483112, -8.002597937117323923, -230.2267818776996080 ) ) ;
#11518 = CARTESIAN_POINT ( 'NONE',  ( 12.81769551943392393, 4.437328497131001193, -221.7762769673541072 ) ) ;
#11519 = CARTESIAN_POINT ( 'NONE',  ( -2.508488193221233953, 16.03207605874066033, -217.8880952293912969 ) ) ;
#11520 = EDGE_CURVE ( 'NONE', #7856, #161, #18114, .T. ) ;
#11521 = CARTESIAN_POINT ( 'NONE',  ( -18.96646980336054611, -22.16549408654085696, -227.7928771762007329 ) ) ;
#11522 = CARTESIAN_POINT ( 'NONE',  ( -14.29986196492902550, 0.06805469746732484282, -227.4167624117703213 ) ) ;
#11523 = CARTESIAN_POINT ( 'NONE',  ( 0.000000000000000000, 0.000000000000000000, 92.00000000000000000 ) ) ;
#11524 = CARTESIAN_POINT ( 'NONE',  ( 17.00168025137501004, 6.212099629982537508, -219.0548246536471595 ) ) ;
#11525 = CARTESIAN_POINT ( 'NONE',  ( 23.84477361619719105, -14.51625201957343592, -224.2863126538025540 ) ) ;
#11526 = CARTESIAN_POINT ( 'NONE',  ( -21.66803296057637951, 19.04503900041684616, -222.6603677762044526 ) ) ;
#11527 = CARTESIAN_POINT ( 'NONE',  ( -5.525229149912007642, -13.32411127922494742, -220.4018445532201440 ) ) ;
#11528 = CARTESIAN_POINT ( 'NONE',  ( 20.76808360334631232, 5.412616674732960931, -234.1222385626545304 ) ) ;
#11529 = CARTESIAN_POINT ( 'NONE',  ( 4.849508625227819003, 24.02665844953846275, -214.9607406399067315 ) ) ;
#11530 = ORIENTED_EDGE ( 'NONE', *, *, #13312, .T. ) ;
#11531 = CARTESIAN_POINT ( 'NONE',  ( -11.26857159993117996, 28.96895336474501192, -225.6039696848669678 ) ) ;
#11532 = CARTESIAN_POINT ( 'NONE',  ( -21.94776718874828347, -0.4748437386657700099, -216.1214812709574176 ) ) ;
#11533 = CARTESIAN_POINT ( 'NONE',  ( -24.96757326990382708, -1.314646799225510199, 9.918699822820977730 ) ) ;
#11534 = CARTESIAN_POINT ( 'NONE',  ( 0.000000000000000000, -23.00000000000000000, 75.00000000000000000 ) ) ;
#11535 = CARTESIAN_POINT ( 'NONE',  ( -3.755296588130283553, 23.77975947300719284, -233.7323173085780752 ) ) ;
#11536 = CARTESIAN_POINT ( 'NONE',  ( -10.76360437932642533, -14.08317586560949408, -234.4387784497120890 ) ) ;
#11537 = CARTESIAN_POINT ( 'NONE',  ( 7.088126259304779353, -19.25156530781288566, -233.7785425911077937 ) ) ;
#11538 = CARTESIAN_POINT ( 'NONE',  ( 15.02813183614916781, -2.406088413402002413, -227.6705652927927872 ) ) ;
#11539 = CARTESIAN_POINT ( 'NONE',  ( -10.52776196018457711, 13.57482816453351937, -219.2327734183297423 ) ) ;
#11540 = CARTESIAN_POINT ( 'NONE',  ( 16.01130065545721592, 20.79417322911648114, -220.9619135886794652 ) ) ;
#11541 = CARTESIAN_POINT ( 'NONE',  ( 15.34286276367735979, 1.557318373440422565, -222.4358706187587416 ) ) ;
#11542 = CARTESIAN_POINT ( 'NONE',  ( -13.71158422780231056, 12.21432067443984693, -232.9166272955793033 ) ) ;
#11543 = CARTESIAN_POINT ( 'NONE',  ( -20.58582428111024853, -15.24952116403520463, -229.8418230779359135 ) ) ;
#11544 = ORIENTED_EDGE ( 'NONE', *, *, #5651, .F. ) ;
#11545 = EDGE_CURVE ( 'NONE', #12391, #15108, #18795, .T. ) ;
#11546 = CARTESIAN_POINT ( 'NONE',  ( -4.334015487506815312, 18.19775486192265390, -231.4387392399519285 ) ) ;
#11547 = CARTESIAN_POINT ( 'NONE',  ( 14.00715608756928532, 4.299235856235253728, -230.2440235370780215 ) ) ;
#11548 = CARTESIAN_POINT ( 'NONE',  ( -2.047892494109819328, 12.88402507277750786, -223.5104301352110951 ) ) ;
#11549 = CARTESIAN_POINT ( 'NONE',  ( 20.33239098169031323, -9.013719117183370599, -216.4483480702011775 ) ) ;
#11550 = DIRECTION ( 'NONE',  ( 0.000000000000000000, 0.000000000000000000, -1.000000000000000000 ) ) ;
#11551 = ORIENTED_EDGE ( 'NONE', *, *, #440, .T. ) ;
#11552 = CARTESIAN_POINT ( 'NONE',  ( -14.83974801774860630, 13.71714848582103485, -216.0935642439352762 ) ) ;
#11553 = CARTESIAN_POINT ( 'NONE',  ( -8.507187218596966360, -16.39771659352221533, -216.5221606441677977 ) ) ;
#11554 = DIRECTION ( 'NONE',  ( -1.000000000000000000, 0.000000000000000000, 0.000000000000000000 ) ) ;
#11555 = CARTESIAN_POINT ( 'NONE',  ( 9.586902571418640662, 24.43292817174309661, -231.9968623198229807 ) ) ;
#11556 = CARTESIAN_POINT ( 'NONE',  ( 2.465190328815661892E-29, 25.00000000000012790, -75.00000000000000000 ) ) ;
#11557 = DIRECTION ( 'NONE',  ( 0.000000000000000000, 0.000000000000000000, 1.000000000000000000 ) ) ;
#11558 = CARTESIAN_POINT ( 'NONE',  ( -16.28135616697389310, 20.98764039357472200, -216.9434553755565958 ) ) ;
#11559 = CARTESIAN_POINT ( 'NONE',  ( 15.21408433160105034, 3.021350230896802103, -222.3056493717910769 ) ) ;
#11560 = AXIS2_PLACEMENT_3D ( 'NONE', #10097, #9989, #22133 ) ;
#11561 = CARTESIAN_POINT ( 'NONE',  ( -23.84293592645385473, 7.532792288779332601, -6.608927698841862153 ) ) ;
#11562 = CARTESIAN_POINT ( 'NONE',  ( 27.75679124201660741, 4.911524026080384075, -221.4430403652340829 ) ) ;
#11563 = CARTESIAN_POINT ( 'NONE',  ( -20.26851768784797869, -0.8260594303982465858, -217.1279713726092098 ) ) ;
#11564 = CARTESIAN_POINT ( 'NONE',  ( 22.26090851979669338, -3.689523054771738586, -218.9825289563843285 ) ) ;
#11565 = CARTESIAN_POINT ( 'NONE',  ( -13.72709560065558421, -5.132649126379569715, -227.9317987811764965 ) ) ;
#11566 = DIRECTION ( 'NONE',  ( 0.000000000000000000, 0.000000000000000000, -1.000000000000000000 ) ) ;
#11567 = AXIS2_PLACEMENT_3D ( 'NONE', #14471, #5902, #6233 ) ;
#11568 = FACE_OUTER_BOUND ( 'NONE', #11398, .T. ) ;
#11569 = CARTESIAN_POINT ( 'NONE',  ( 4.238595127209166868, 26.19205419861516404, -230.1142052665570077 ) ) ;
#11570 = CARTESIAN_POINT ( 'NONE',  ( 10.42186625103445152, -25.39807580958450473, -217.7675295214572202 ) ) ;
#11571 = CARTESIAN_POINT ( 'NONE',  ( 15.10937218716165020, -26.44221868192832758, -222.7999243300199907 ) ) ;
#11572 = CARTESIAN_POINT ( 'NONE',  ( -25.44919589272258520, 4.740781954932180575, -232.0725131810460766 ) ) ;
#11573 = CARTESIAN_POINT ( 'NONE',  ( 20.05202556141620107, 8.012988804822112954, -215.8722494878839200 ) ) ;
#11574 = CARTESIAN_POINT ( 'NONE',  ( 28.46362550855882745, 7.392895870364313282, -223.4682258299149566 ) ) ;
#11575 = ORIENTED_EDGE ( 'NONE', *, *, #2672, .T. ) ;
#11576 = CARTESIAN_POINT ( 'NONE',  ( 3.436191426816104233, -15.97976940388950773, -231.4631329546418499 ) ) ;
#11577 = CARTESIAN_POINT ( 'NONE',  ( 7.157650466794455824, -8.055668064929562888, 92.00000000000001421 ) ) ;
#11578 = CARTESIAN_POINT ( 'NONE',  ( -29.15345109632842124, 14.07532767497844262, -225.0972140442887621 ) ) ;
#11579 = AXIS2_PLACEMENT_3D ( 'NONE', #17290, #21098, #2195 ) ;
#11580 = CARTESIAN_POINT ( 'NONE',  ( 20.05374812456133782, 24.17492691056345677, -223.1494843338164458 ) ) ;
#11581 = CARTESIAN_POINT ( 'NONE',  ( 4.024086222410633518, 12.48004227094270746, -230.0177668608922374 ) ) ;
#11582 = CARTESIAN_POINT ( 'NONE',  ( 14.12786214016513675, -4.771276416369937046, -223.8547069812204029 ) ) ;
#11583 = CARTESIAN_POINT ( 'NONE',  ( -7.395406416482832590, 12.93623984139929739, -219.2606224730616873 ) ) ;
#11584 = CARTESIAN_POINT ( 'NONE',  ( -13.65925618638770800, 3.289586759644148817, -222.1579143493116533 ) ) ;
#11585 = EDGE_CURVE ( 'NONE', #20364, #16045, #5868, .T. ) ;
#11586 = AXIS2_PLACEMENT_3D ( 'NONE', #19118, #5274, #343 ) ;
#11587 = CARTESIAN_POINT ( 'NONE',  ( 5.030854775705693172, 19.94152319263364603, -234.9034581965229336 ) ) ;
#11588 = CARTESIAN_POINT ( 'NONE',  ( -22.18165477997343871, 9.502253276305026475, -218.0070055737419636 ) ) ;
#11589 = CARTESIAN_POINT ( 'NONE',  ( -6.201839134465864767, 11.37481922992157379, -223.7040893475979146 ) ) ;
#11590 = CARTESIAN_POINT ( 'NONE',  ( 0.1824719560092671056, 10.76782065184847959, 92.00000000000001421 ) ) ;
#11591 = CARTESIAN_POINT ( 'NONE',  ( 3.746955526231565248, 25.82691596581962656, -220.7780764774678062 ) ) ;
#11592 = CARTESIAN_POINT ( 'NONE',  ( 28.36095019830170472, -8.296631283839911220, -225.2861439608085448 ) ) ;
#11593 = DIRECTION ( 'NONE',  ( -1.000000000000000000, 0.000000000000000000, 2.891205793294678696E-17 ) ) ;
#11594 = CARTESIAN_POINT ( 'NONE',  ( 1.322875655532295136, 1.500000000000000000, -120.0000000000000142 ) ) ;
#11595 = CARTESIAN_POINT ( 'NONE',  ( 22.02796522526679723, 16.41909032291435366, -220.1590600991317217 ) ) ;
#11596 = CARTESIAN_POINT ( 'NONE',  ( -11.58793217866213787, -13.88438693436061477, -219.4860661588769801 ) ) ;
#11597 = AXIS2_PLACEMENT_3D ( 'NONE', #12476, #16072, #4008 ) ;
#11598 = LINE ( 'NONE', #9804, #13897 ) ;
#11599 = CIRCLE ( 'NONE', #13053, 10.00000000000000000 ) ;
#11600 = CARTESIAN_POINT ( 'NONE',  ( -8.857704405076667342, 24.20848540845601704, -218.8859504303524091 ) ) ;
#11601 = SURFACE_SIDE_STYLE ('',( #1587 ) ) ;
#11602 = CARTESIAN_POINT ( 'NONE',  ( 17.93010821528303822, -10.80507700282924688, -233.3968735006674251 ) ) ;
#11603 = CARTESIAN_POINT ( 'NONE',  ( 13.17768061945195157, 6.810183613937965674, -219.8302315341053657 ) ) ;
#11604 = CARTESIAN_POINT ( 'NONE',  ( -4.334015487506815312, 18.19775486192265390, -231.4387392399519285 ) ) ;
#11605 = CARTESIAN_POINT ( 'NONE',  ( -9.290933312444883185, 29.15551353946876745, -225.8551562993724247 ) ) ;
#11606 = ORIENTED_EDGE ( 'NONE', *, *, #7297, .T. ) ;
#11607 = CARTESIAN_POINT ( 'NONE',  ( -16.47483915600249205, -3.991485801086211538, -222.0851216934102297 ) ) ;
#11608 = CARTESIAN_POINT ( 'NONE',  ( -21.28804099221702018, -0.9277163183344186992, -219.0000000002572733 ) ) ;
#11609 = DIRECTION ( 'NONE',  ( 0.000000000000000000, 0.000000000000000000, 1.000000000000000000 ) ) ;
#11610 = CARTESIAN_POINT ( 'NONE',  ( -30.26911233660276679, -7.575179034252494503, -222.6017624672529109 ) ) ;
#11611 = CARTESIAN_POINT ( 'NONE',  ( 22.20554449732931346, 18.01468431515759860, -218.9348803756412849 ) ) ;
#11612 = CARTESIAN_POINT ( 'NONE',  ( -27.28038240442402440, 5.683827137705129040, -226.0726697751923382 ) ) ;
#11613 = VECTOR ( 'NONE', #5592, 1000.000000000000227 ) ;
#11614 = CARTESIAN_POINT ( 'NONE',  ( -4.974038791218384326, 28.61915055369004079, -219.5057940952933961 ) ) ;
#11615 = CARTESIAN_POINT ( 'NONE',  ( 15.33651282626308010, 7.807290788239344970, -218.6940806506825652 ) ) ;
#11616 = VERTEX_POINT ( 'NONE', #18901 ) ;
#11617 = CARTESIAN_POINT ( 'NONE',  ( -9.514686225151438137, -9.899715435889788751, -219.6589915062491229 ) ) ;
#11618 = ORIENTED_EDGE ( 'NONE', *, *, #15930, .F. ) ;
#11619 = CARTESIAN_POINT ( 'NONE',  ( -13.02663300398358892, -17.15584419188240162, -232.5492131852532793 ) ) ;
#11620 = EDGE_CURVE ( 'NONE', #846, #10588, #3806, .T. ) ;
#11621 = CARTESIAN_POINT ( 'NONE',  ( -13.55637112341987383, 4.614880311503475774, -231.8130385267184010 ) ) ;
#11622 = CARTESIAN_POINT ( 'NONE',  ( 8.649266908999912573, -10.50942778440553482, -226.4415026780416440 ) ) ;
#11623 = CARTESIAN_POINT ( 'NONE',  ( 23.77009720158773831, -0.5966687509537305090, -216.6384684467892043 ) ) ;
#11624 = CARTESIAN_POINT ( 'NONE',  ( -21.80830016239255897, -4.781675611938959847, -217.4666014280278148 ) ) ;
#11625 = CARTESIAN_POINT ( 'NONE',  ( 20.85755584069816493, 20.53615333921957742, -227.2010381488614996 ) ) ;
#11626 = CARTESIAN_POINT ( 'NONE',  ( 0.000000000000000000, 0.000000000000000000, -78.50000000000000000 ) ) ;
#11627 = CARTESIAN_POINT ( 'NONE',  ( -27.40681729237160269, 15.04232492504307572, -225.3323746796125704 ) ) ;
#11628 = CARTESIAN_POINT ( 'NONE',  ( 16.97369223523349646, 15.19068754808448851, -217.0779026324121332 ) ) ;
#11629 = CARTESIAN_POINT ( 'NONE',  ( 12.85408565574548412, 7.821283853063205171, -223.1248833997948111 ) ) ;
#11630 = CARTESIAN_POINT ( 'NONE',  ( 12.11771628698343051, 17.56545729485151952, -218.0322663566023493 ) ) ;
#11631 = CARTESIAN_POINT ( 'NONE',  ( 11.14866046433140490, -17.10865642060806024, -235.2771047445726822 ) ) ;
#11632 = AXIS2_PLACEMENT_3D ( 'NONE', #15497, #20538, #17410 ) ;
#11633 = AXIS2_PLACEMENT_3D ( 'NONE', #19314, #2425, #11101 ) ;
#11634 = CARTESIAN_POINT ( 'NONE',  ( -13.01542355754912172, 26.77630951171455820, -225.1545229496516356 ) ) ;
#11635 = CARTESIAN_POINT ( 'NONE',  ( 0.000000000000000000, 0.000000000000000000, -24.99999999999999645 ) ) ;
#11636 = CARTESIAN_POINT ( 'NONE',  ( 0.000000000000000000, -23.00000000000006040, -69.99999999999998579 ) ) ;
#11637 = CARTESIAN_POINT ( 'NONE',  ( 14.73698509926073186, 4.443590625350892331, -227.4062002049096236 ) ) ;
#11638 = CARTESIAN_POINT ( 'NONE',  ( 7.357019007885960526, -24.37006613449481662, -217.4041786725384782 ) ) ;
#11639 = CARTESIAN_POINT ( 'NONE',  ( -18.74633356284308761, 11.17209001323738704, -217.5809474206552068 ) ) ;
#11640 = CARTESIAN_POINT ( 'NONE',  ( -3.996294969088721505, 28.80481464818193515, -222.8623509149411746 ) ) ;
#11641 = CARTESIAN_POINT ( 'NONE',  ( -13.33530847390368024, -5.065163879519744228, -226.5386329521395226 ) ) ;
#11642 = CARTESIAN_POINT ( 'NONE',  ( 14.50618777373884960, 4.375057440872940795, -230.8807389798650433 ) ) ;
#11643 = CARTESIAN_POINT ( 'NONE',  ( 7.803634760976553508, 10.78293796201124266, -229.6314106675118865 ) ) ;
#11644 = ORIENTED_EDGE ( 'NONE', *, *, #1994, .T. ) ;
#11645 = CARTESIAN_POINT ( 'NONE',  ( 1.382955251742491898, 16.46353944795171032, -231.7743150979565030 ) ) ;
#11646 = CARTESIAN_POINT ( 'NONE',  ( 13.86395146404758982, -8.823451364178625411, -228.3963352256065491 ) ) ;
#11647 = CARTESIAN_POINT ( 'NONE',  ( -23.05940187647296469, -9.657892124444725113, -2.614105026375423524 ) ) ;
#11648 = FACE_OUTER_BOUND ( 'NONE', #10259, .T. ) ;
#11649 = AXIS2_PLACEMENT_3D ( 'NONE', #527, #17863, #14599 ) ;
#11650 = CARTESIAN_POINT ( 'NONE',  ( 4.389496648589924277, 14.47660514356954131, -220.6151178996808540 ) ) ;
#11651 = CARTESIAN_POINT ( 'NONE',  ( -3.739406429132753562, -13.42303118918103344, -219.1969888661882635 ) ) ;
#11652 = CARTESIAN_POINT ( 'NONE',  ( 15.34510829589250491, -24.56813251781886009, -230.1307231235174982 ) ) ;
#11653 = CARTESIAN_POINT ( 'NONE',  ( 10.40291689048662782, -13.87512507945592333, -231.9656913702303029 ) ) ;
#11654 = CARTESIAN_POINT ( 'NONE',  ( -19.01002492504315811, 19.85266905124972681, -219.0021410556803687 ) ) ;
#11655 = CARTESIAN_POINT ( 'NONE',  ( 5.791579991237209235, 15.48299465423324861, -228.0203551130359472 ) ) ;
#11656 = CARTESIAN_POINT ( 'NONE',  ( -15.23434562258889891, -0.4010941804143903222, -220.4743703065900036 ) ) ;
#11657 = CARTESIAN_POINT ( 'NONE',  ( -12.39654240422350462, 9.886262337642440556, -219.1620329226848014 ) ) ;
#11658 = CARTESIAN_POINT ( 'NONE',  ( -16.29786170208491924, -8.453292648900102790, -230.0691174225123632 ) ) ;
#11659 = ORIENTED_EDGE ( 'NONE', *, *, #5375, .T. ) ;
#11660 = CARTESIAN_POINT ( 'NONE',  ( -7.873497077133136735, 15.44270125396616677, -230.2562282217168672 ) ) ;
#11661 = CARTESIAN_POINT ( 'NONE',  ( 21.72366288329714834, 2.385777479048636351, -215.9150265590827757 ) ) ;
#11662 = CARTESIAN_POINT ( 'NONE',  ( -5.727886109716582297, 15.25217619989539486, -230.5419623196804650 ) ) ;
#11663 = CARTESIAN_POINT ( 'NONE',  ( 13.09169075717699293, -6.869491136113572871, -220.8313809912125691 ) ) ;
#11664 = LINE ( 'NONE', #1421, #15051 ) ;
#11665 = EDGE_LOOP ( 'NONE', ( #6850, #1043, #2191, #21088, #736, #19983 ) ) ;
#11666 = CARTESIAN_POINT ( 'NONE',  ( -15.82069055112642353, 8.315535108674763976, -217.2800172218543935 ) ) ;
#11667 = CARTESIAN_POINT ( 'NONE',  ( -26.63259355655987548, -7.256793811979244779, -216.2488627322786101 ) ) ;
#11668 = DIRECTION ( 'NONE',  ( -1.000000000000000000, 0.000000000000000000, 0.000000000000000000 ) ) ;
#11669 = MECHANICAL_DESIGN_GEOMETRIC_PRESENTATION_REPRESENTATION (  '', ( #19924 ), #1961 ) ;
#11670 = CARTESIAN_POINT ( 'NONE',  ( 7.762960416026701616, 12.60702317161859121, -221.9096828323375235 ) ) ;
#11671 = CARTESIAN_POINT ( 'NONE',  ( 0.000000000000000000, 0.000000000000000000, -75.00000000000000000 ) ) ;
#11672 = PRODUCT_DEFINITION_CONTEXT ( 'detailed design', #15204, 'design' ) ;
#11673 = CARTESIAN_POINT ( 'NONE',  ( 13.36656406724190305, -19.73987914515934960, -233.3798509643240209 ) ) ;
#11674 = SURFACE_SIDE_STYLE ('',( #20202 ) ) ;
#11675 = CARTESIAN_POINT ( 'NONE',  ( -16.63766460830045091, 5.158675778507696208, -232.1659425527909093 ) ) ;
#11676 = CARTESIAN_POINT ( 'NONE',  ( -14.30586181932858914, 18.69563132175512266, -215.8217153853723573 ) ) ;
#11677 = CARTESIAN_POINT ( 'NONE',  ( 22.44730228620155899, 3.608729811217749717, -232.0798239124179645 ) ) ;
#11678 = CARTESIAN_POINT ( 'NONE',  ( -6.507186921339367380, -21.94905981650347826, -217.8194053188079238 ) ) ;
#11679 = CARTESIAN_POINT ( 'NONE',  ( -23.28348052659234924, 9.104820739214817493, -4.148323561781968927 ) ) ;
#11680 = CARTESIAN_POINT ( 'NONE',  ( 16.00819137755116373, 4.595691552992191120, -229.5669508871464757 ) ) ;
#11681 = CARTESIAN_POINT ( 'NONE',  ( 0.000000000000000000, 23.00000000000006040, 75.00000000000000000 ) ) ;
#11682 = CARTESIAN_POINT ( 'NONE',  ( 22.49864633775863609, -6.670857247392108391, -230.7634588385486438 ) ) ;
#11683 = CARTESIAN_POINT ( 'NONE',  ( -24.15031621174628285, -13.05338392360020627, -219.0842748323915714 ) ) ;
#11684 = CARTESIAN_POINT ( 'NONE',  ( -20.96199077856121207, -9.466050238387317961, 3.240634028981310255 ) ) ;
#11685 = CARTESIAN_POINT ( 'NONE',  ( -17.50000000000000711, 0.000000000000000000, -55.00000000000000000 ) ) ;
#11686 = CARTESIAN_POINT ( 'NONE',  ( 5.466128392039544259, 27.94759090250835243, -223.5617905851570981 ) ) ;
#11687 = CARTESIAN_POINT ( 'NONE',  ( 5.503098680704820111, -17.53359096179937993, -217.0817822229213618 ) ) ;
#11688 = CIRCLE ( 'NONE', #7745, 17.50000000000007816 ) ;
#11689 = CARTESIAN_POINT ( 'NONE',  ( 10.10435529162921853, -13.32996982371095918, -231.5224098423250894 ) ) ;
#11690 = ORIENTED_EDGE ( 'NONE', *, *, #8288, .T. ) ;
#11691 = COLOUR_RGB ( '', 0.09019608, 0.27058824, 0.51372549) ;
#11692 = CARTESIAN_POINT ( 'NONE',  ( -16.57767831947938575, 23.50485984366324388, -222.7977068309636763 ) ) ;
#11693 = CARTESIAN_POINT ( 'NONE',  ( -17.64438593497130370, 2.824953307685432069, -229.4443205246391813 ) ) ;
#11694 = CARTESIAN_POINT ( 'NONE',  ( 14.04819512851487673, 6.831178966487911453, -222.6676118107292552 ) ) ;
#11695 = ORIENTED_EDGE ( 'NONE', *, *, #4428, .T. ) ;
#11696 = CARTESIAN_POINT ( 'NONE',  ( -13.60885102855131201, -21.92822159330905762, -220.4851091041354607 ) ) ;
#11697 = CARTESIAN_POINT ( 'NONE',  ( 3.593890535426114141, -10.35670734540880922, 92.00000000000000000 ) ) ;
#11698 = CARTESIAN_POINT ( 'NONE',  ( -26.12939716039095117, 11.33146045174629357, -233.1192402782019997 ) ) ;
#11699 = CARTESIAN_POINT ( 'NONE',  ( 8.730612144237051453, 13.93563980088501886, -217.1627566045470132 ) ) ;
#11700 = CARTESIAN_POINT ( 'NONE',  ( 11.43327405580198608, -14.46863304034511799, -220.4355838810013495 ) ) ;
#11701 = CARTESIAN_POINT ( 'NONE',  ( 5.343558017910363667, 26.29639771561252459, -218.1010331760174665 ) ) ;
#11702 = CARTESIAN_POINT ( 'NONE',  ( -28.59157645096996347, 5.137867505054540374, -220.4667042235044505 ) ) ;
#11703 = CARTESIAN_POINT ( 'NONE',  ( 5.179557175392591972, 10.46258103618983881, -224.6216839350439614 ) ) ;
#11704 = AXIS2_PLACEMENT_3D ( 'NONE', #6334, #16693, #14574 ) ;
#11705 = CARTESIAN_POINT ( 'NONE',  ( -21.93223149637851677, 1.726402211042445067, -231.1052103444381203 ) ) ;
#11706 = CARTESIAN_POINT ( 'NONE',  ( -14.73016414256368911, 22.23431809695627237, -217.1425123644553707 ) ) ;
#11707 = DIRECTION ( 'NONE',  ( 1.000000000000000000, 0.000000000000000000, 0.000000000000000000 ) ) ;
#11708 = CARTESIAN_POINT ( 'NONE',  ( 2.021807401899061496, 24.17554150923399092, -230.4042646614662146 ) ) ;
#11709 = FACE_OUTER_BOUND ( 'NONE', #10199, .T. ) ;
#11710 = DIRECTION ( 'NONE',  ( -6.982962677686272233E-15, 1.000000000000000000, 0.000000000000000000 ) ) ;
#11711 = CARTESIAN_POINT ( 'NONE',  ( -26.22594988380878789, -0.1068133454905619700, -219.1167922977186322 ) ) ;
#11712 = CARTESIAN_POINT ( 'NONE',  ( 16.07305932912010960, 0.9253679043337685872, -229.0409936706996064 ) ) ;
#11713 = CARTESIAN_POINT ( 'NONE',  ( -13.39502153392024475, -9.880902914596246589, -222.0112808355889342 ) ) ;
#11714 = DIRECTION ( 'NONE',  ( -0.000000000000000000, -0.000000000000000000, -1.000000000000000000 ) ) ;
#11715 = EDGE_CURVE ( 'NONE', #17015, #8742, #6240, .T. ) ;
#11716 = CARTESIAN_POINT ( 'NONE',  ( -4.466732464217805898, 19.42663028452474450, -231.9485309169485561 ) ) ;
#11717 = CARTESIAN_POINT ( 'NONE',  ( 2.641673488600395636, -17.65289918763021149, -219.1873688300129288 ) ) ;
#11718 = CARTESIAN_POINT ( 'NONE',  ( 16.97369223523349646, 15.19068754808448851, -217.0779026324121332 ) ) ;
#11719 = CARTESIAN_POINT ( 'NONE',  ( -7.375127652145912371, 13.01042140126078195, -223.9959097520547004 ) ) ;
#11720 = CARTESIAN_POINT ( 'NONE',  ( -8.653738780971721667, 11.12943719949617893, -219.7525355316396087 ) ) ;
#11721 = ORIENTED_EDGE ( 'NONE', *, *, #13389, .F. ) ;
#11722 = CARTESIAN_POINT ( 'NONE',  ( 19.51310828881794990, -1.786742129898636344, -215.1201286626718741 ) ) ;
#11723 = VECTOR ( 'NONE', #1667, 1000.000000000000000 ) ;
#11724 = CARTESIAN_POINT ( 'NONE',  ( 15.85665641241444668, 18.24713744004561988, -217.7195292979064902 ) ) ;
#11725 = VECTOR ( 'NONE', #4616, 1000.000000000000000 ) ;
#11726 = CARTESIAN_POINT ( 'NONE',  ( -15.10760069511485604, 3.026516874529453283, -224.5685390982118861 ) ) ;
#11727 = CARTESIAN_POINT ( 'NONE',  ( -26.70018640714903668, 3.110792036746048428, -228.8761207540193823 ) ) ;
#11728 = FACE_OUTER_BOUND ( 'NONE', #10205, .T. ) ;
#11729 = CARTESIAN_POINT ( 'NONE',  ( -17.70471257751854921, -0.5540196600081067624, -232.9322037287452360 ) ) ;
#11730 = CARTESIAN_POINT ( 'NONE',  ( 8.592982993077152187, 10.20906991731218838, -226.0923132092261483 ) ) ;
#11731 = CARTESIAN_POINT ( 'NONE',  ( -13.91323058514953637, 8.006348396443080162, -225.5064972756604220 ) ) ;
#11732 = CARTESIAN_POINT ( 'NONE',  ( 2.165130313308041288, 31.55305250914585002, -225.6791154433767304 ) ) ;
#11733 = CARTESIAN_POINT ( 'NONE',  ( 13.14260364752544596, 5.866423290307341887, -222.7705901084601408 ) ) ;
#11734 = AXIS2_PLACEMENT_3D ( 'NONE', #9693, #21491, #14549 ) ;
#11735 = ORIENTED_EDGE ( 'NONE', *, *, #10351, .T. ) ;
#11736 = CARTESIAN_POINT ( 'NONE',  ( -11.58651333402397476, -12.19597367159924595, -216.5418320517508448 ) ) ;
#11737 = ORIENTED_EDGE ( 'NONE', *, *, #16835, .T. ) ;
#11738 = CARTESIAN_POINT ( 'NONE',  ( -10.39692419770002552, -10.11462123336039021, -222.6538761800393047 ) ) ;
#11739 = CARTESIAN_POINT ( 'NONE',  ( -16.81617677814535128, 0.6259372974186930838, -233.5115673467681745 ) ) ;
#11740 = CARTESIAN_POINT ( 'NONE',  ( 10.30328786010431052, -20.08430705480546408, -216.1847100135515802 ) ) ;
#11741 = CARTESIAN_POINT ( 'NONE',  ( 13.79223148755288797, -4.990905483784310981, -230.8248327435212559 ) ) ;
#11742 = CARTESIAN_POINT ( 'NONE',  ( -28.30937415889876618, -7.921132361018833556, -222.9755670691803857 ) ) ;
#11743 = EDGE_CURVE ( 'NONE', #9103, #8796, #21525, .T. ) ;
#11744 = CARTESIAN_POINT ( 'NONE',  ( 21.46274988498219471, 20.25395488059580984, -223.1777011585387243 ) ) ;
#11745 = AXIS2_PLACEMENT_3D ( 'NONE', #7939, #6238, #18182 ) ;
#11746 =( NAMED_UNIT ( * ) SI_UNIT ( $, .STERADIAN. ) SOLID_ANGLE_UNIT ( ) );
#11747 = CARTESIAN_POINT ( 'NONE',  ( -25.00745438246740804, 14.90779342625281778, -219.2410538611701156 ) ) ;
#11748 = CARTESIAN_POINT ( 'NONE',  ( 20.88350594575732799, 13.65521425050155813, -232.8060468608549911 ) ) ;
#11749 = CARTESIAN_POINT ( 'NONE',  ( 7.762960416026701616, 12.60702317161859121, -221.9096828323375235 ) ) ;
#11750 = CARTESIAN_POINT ( 'NONE',  ( 10.64798096806036121, 19.48085866535796740, -231.3996658690317361 ) ) ;
#11751 = CARTESIAN_POINT ( 'NONE',  ( 21.94513595990333954, -23.27941424421253203, -222.2428713697011631 ) ) ;
#11752 = CARTESIAN_POINT ( 'NONE',  ( -5.836418080594380164, 30.19240250712089590, -223.8354869487762357 ) ) ;
#11753 = CARTESIAN_POINT ( 'NONE',  ( -29.30406754532526037, 5.063969254119831120, -221.8212091093853076 ) ) ;
#11754 = DIRECTION ( 'NONE',  ( 0.000000000000000000, 0.000000000000000000, 1.000000000000000000 ) ) ;
#11755 = CARTESIAN_POINT ( 'NONE',  ( 13.12488928717151637, 1.607335365469798272E-15, -99.99999999999998579 ) ) ;
#11756 = CARTESIAN_POINT ( 'NONE',  ( 7.808093059109005196, -25.57408461116448706, -218.1679985877120487 ) ) ;
#11757 = CARTESIAN_POINT ( 'NONE',  ( -12.05423124486310904, 12.38527783110887803, -219.7419643105747014 ) ) ;
#11758 = EDGE_CURVE ( 'NONE', #21649, #14946, #20800, .T. ) ;
#11759 = CARTESIAN_POINT ( 'NONE',  ( 4.303123380281038024, 17.66787810618728827, -231.9745698734655832 ) ) ;
#11760 = CARTESIAN_POINT ( 'NONE',  ( -22.23616899077527975, -11.51447210886970751, -217.5950109096934568 ) ) ;
#11761 = CARTESIAN_POINT ( 'NONE',  ( -26.35007260221545877, 6.140745174321167177, -221.9336216792591188 ) ) ;
#11762 = EDGE_CURVE ( 'NONE', #19351, #1956, #12715, .T. ) ;
#11763 = CARTESIAN_POINT ( 'NONE',  ( 17.04685026979186446, 18.05617612716381970, -216.0910122987878310 ) ) ;
#11764 = ORIENTED_EDGE ( 'NONE', *, *, #9228, .F. ) ;
#11765 = CARTESIAN_POINT ( 'NONE',  ( 0.2389779871941385414, 16.64595486589868045, -218.1658233406367629 ) ) ;
#11766 = CARTESIAN_POINT ( 'NONE',  ( 17.47462908134004422, -13.97354901070533906, -218.8807045398700666 ) ) ;
#11767 = CARTESIAN_POINT ( 'NONE',  ( 20.07985072697885442, -15.33367264652052953, -217.4666949641080294 ) ) ;
#11768 = CARTESIAN_POINT ( 'NONE',  ( -2.100000000000000089, 2.571758278209441957E-16, -126.0000000000000284 ) ) ;
#11769 = CARTESIAN_POINT ( 'NONE',  ( 4.543450689403089271, 15.91052110650461771, -218.9437823786444426 ) ) ;
#11770 = CARTESIAN_POINT ( 'NONE',  ( -15.94006964721192432, -5.209069452486915885, -233.2212940081757040 ) ) ;
#11771 = CARTESIAN_POINT ( 'NONE',  ( -1.778254167844783851, -12.78790610364390012, -225.9413532495922254 ) ) ;
#11772 = CARTESIAN_POINT ( 'NONE',  ( 13.47054497134856277, -24.75371201277411615, -218.7687119198782000 ) ) ;
#11773 = CARTESIAN_POINT ( 'NONE',  ( -15.33438615632468149, 23.56248205204123991, -229.2747191038674544 ) ) ;
#11774 = CARTESIAN_POINT ( 'NONE',  ( 8.539351012053531420, 16.03230746435535181, -220.6282946404833751 ) ) ;
#11775 = CARTESIAN_POINT ( 'NONE',  ( -14.68037037322036475, 3.441677802729143920, -220.1396515630443389 ) ) ;
#11776 = CARTESIAN_POINT ( 'NONE',  ( -9.982417347796181062, 8.907629238417765549, -225.5124013436514474 ) ) ;
#11777 = CARTESIAN_POINT ( 'NONE',  ( -15.17770002056818868, -9.429316640439420638, -220.2566215541993699 ) ) ;
#11778 = ORIENTED_EDGE ( 'NONE', *, *, #12038, .F. ) ;
#11779 = CARTESIAN_POINT ( 'NONE',  ( -9.233762381136051189, 19.18161952504991419, -232.0796851897838451 ) ) ;
#11780 = CARTESIAN_POINT ( 'NONE',  ( 12.25122766587143630, 4.035812653434439845, -225.7709573147497224 ) ) ;
#11781 = CARTESIAN_POINT ( 'NONE',  ( 8.373295497769937867, 8.203271496719947820, -226.1884629658694053 ) ) ;
#11782 = CARTESIAN_POINT ( 'NONE',  ( 12.44471834243122466, -10.90083019301730083, -219.2211511521849161 ) ) ;
#11783 = DIRECTION ( 'NONE',  ( -1.000000000000000000, 0.000000000000000000, 0.000000000000000000 ) ) ;
#11784 = ORIENTED_EDGE ( 'NONE', *, *, #13717, .F. ) ;
#11785 = CARTESIAN_POINT ( 'NONE',  ( -13.55591840520136770, 8.363404288414606924, -231.2690188357804857 ) ) ;
#11786 = CARTESIAN_POINT ( 'NONE',  ( -17.53163374842703703, -10.16025041587072764, -214.8411325589202647 ) ) ;
#11787 = CARTESIAN_POINT ( 'NONE',  ( 0.000000000000000000, 0.000000000000000000, -70.00000000000000000 ) ) ;
#11788 = CARTESIAN_POINT ( 'NONE',  ( 7.639528166734322667, 11.92751229241157596, -224.6077814063189635 ) ) ;
#11789 = CARTESIAN_POINT ( 'NONE',  ( 0.000000000000000000, 0.000000000000000000, 75.00000000000000000 ) ) ;
#11790 = CARTESIAN_POINT ( 'NONE',  ( 21.39922646226391478, -21.53954253117021977, -224.1701659532164967 ) ) ;
#11791 = CARTESIAN_POINT ( 'NONE',  ( -21.93900267957129557, 7.862893636934532360, -233.4951761057262161 ) ) ;
#11792 = CARTESIAN_POINT ( 'NONE',  ( -7.752954785937490989, 10.21341112307795385, -225.5135920495299615 ) ) ;
#11793 = CARTESIAN_POINT ( 'NONE',  ( 15.57986488780344736, -0.6155558446892130942, -225.2777919203616932 ) ) ;
#11794 = CARTESIAN_POINT ( 'NONE',  ( -5.980659577089002532, -19.45286470896024156, -217.9322865582606710 ) ) ;
#11795 = DIRECTION ( 'NONE',  ( -0.000000000000000000, -0.000000000000000000, 1.000000000000000000 ) ) ;
#11796 = CARTESIAN_POINT ( 'NONE',  ( 25.69300549816939494, 5.947472783069708946, -230.6131061331718115 ) ) ;
#11797 = DIRECTION ( 'NONE',  ( -0.000000000000000000, -0.000000000000000000, 1.000000000000000000 ) ) ;
#11798 = CARTESIAN_POINT ( 'NONE',  ( 13.81930941494936782, -14.31252807618095879, -218.6132940872857375 ) ) ;
#11799 = CARTESIAN_POINT ( 'NONE',  ( 12.83912001598358898, -2.984904020217645115, -224.6440377188723687 ) ) ;
#11800 = CARTESIAN_POINT ( 'NONE',  ( -22.03409719845232928, -6.612754814632006095, 7.529125094242241190 ) ) ;
#11801 = CARTESIAN_POINT ( 'NONE',  ( 8.647507700742417924, 16.42978512283924175, -220.3082116258600536 ) ) ;
#11802 = CARTESIAN_POINT ( 'NONE',  ( 11.96323484613444599, -17.37820513000257350, -215.5071828020160183 ) ) ;
#11803 = CARTESIAN_POINT ( 'NONE',  ( 11.43609017326686050, -13.06727081285745307, -217.8903327850316316 ) ) ;
#11804 = VERTEX_POINT ( 'NONE', #10796 ) ;
#11805 = CARTESIAN_POINT ( 'NONE',  ( -21.23733589435050817, 17.25275849955597351, -229.9547908233139708 ) ) ;
#11806 = CARTESIAN_POINT ( 'NONE',  ( 21.72366288329714834, 2.385777479048636351, -215.9150265590827757 ) ) ;
#11807 = CARTESIAN_POINT ( 'NONE',  ( 21.91535456744164279, 7.573568724377624406, -232.0371228855588868 ) ) ;
#11808 = EDGE_LOOP ( 'NONE', ( #218, #3542, #21945, #15473 ) ) ;
#11809 = CARTESIAN_POINT ( 'NONE',  ( -11.18644257538908526, -20.90776414258732174, -230.8249452324125173 ) ) ;
#11810 = CARTESIAN_POINT ( 'NONE',  ( -8.469031667849373335, -6.688043756404093543, 91.99999999999997158 ) ) ;
#11811 = CARTESIAN_POINT ( 'NONE',  ( -17.92628912275201003, -0.6090139417824500523, -215.7724435048976943 ) ) ;
#11812 = CARTESIAN_POINT ( 'NONE',  ( 8.454338299486085617, 13.28844197278511530, -217.6979371188311632 ) ) ;
#11813 = CARTESIAN_POINT ( 'NONE',  ( 20.29455491689504498, -15.47394441642566143, -219.8812143983372778 ) ) ;
#11814 = CARTESIAN_POINT ( 'NONE',  ( 8.496844655769807630, 14.66037471857024599, -219.1631158796573118 ) ) ;
#11815 = CARTESIAN_POINT ( 'NONE',  ( -20.54164754914381064, 7.122791156791981493, -233.5720402887671980 ) ) ;
#11816 = AXIS2_PLACEMENT_3D ( 'NONE', #17286, #5453, #7166 ) ;
#11817 = CARTESIAN_POINT ( 'NONE',  ( 18.26039090677515375, 26.14311541888654844, -228.1864986152887127 ) ) ;
#11818 = CARTESIAN_POINT ( 'NONE',  ( -26.47320305716024791, 9.675235842009668019, -228.3542180911597654 ) ) ;
#11819 = CARTESIAN_POINT ( 'NONE',  ( -2.208416658185406334, 29.10348627872611615, -219.8480645685746424 ) ) ;
#11820 = CARTESIAN_POINT ( 'NONE',  ( -7.549707216296317469, 7.678935899902893603, 91.99999999999998579 ) ) ;
#11821 = CARTESIAN_POINT ( 'NONE',  ( 0.7326557587344989519, -29.96088689026728602, -229.4725774697800205 ) ) ;
#11822 = CARTESIAN_POINT ( 'NONE',  ( 17.00614511541963836, -1.958782916976874233, -219.4638360731791806 ) ) ;
#11823 = CARTESIAN_POINT ( 'NONE',  ( 0.000000000000000000, 0.000000000000000000, -65.00000000000000000 ) ) ;
#11824 = DIRECTION ( 'NONE',  ( -0.000000000000000000, -0.000000000000000000, -1.000000000000000000 ) ) ;
#11825 = CARTESIAN_POINT ( 'NONE',  ( -12.36382104905844592, -0.1264132474004772688, -228.0034406263598896 ) ) ;
#11826 = CARTESIAN_POINT ( 'NONE',  ( -16.98436007432217920, -11.01716238098750544, -231.0196200964405193 ) ) ;
#11827 = CARTESIAN_POINT ( 'NONE',  ( 18.80535572547204026, 2.962702208451975849, -225.4869357187871231 ) ) ;
#11828 = CARTESIAN_POINT ( 'NONE',  ( 9.037704487505543227, -20.74919929927824214, -217.6023494967207625 ) ) ;
#11829 = ADVANCED_FACE ( 'NONE', ( #12151 ), #2233, .T. ) ;
#11830 = CARTESIAN_POINT ( 'NONE',  ( 9.575488824002899690, 13.89846378187365694, -220.1158735840035945 ) ) ;
#11831 = CARTESIAN_POINT ( 'NONE',  ( -4.224287562409271501, 29.03635716824519264, -224.1823526280761882 ) ) ;
#11832 = CARTESIAN_POINT ( 'NONE',  ( -12.22073052649759184, 14.03927388329973525, -215.9097966823721606 ) ) ;
#11833 = ORIENTED_EDGE ( 'NONE', *, *, #1573, .T. ) ;
#11834 = CARTESIAN_POINT ( 'NONE',  ( 31.43562455973156844, -0.2326399569828876968, -228.1442589022926484 ) ) ;
#11835 = ORIENTED_EDGE ( 'NONE', *, *, #16439, .F. ) ;
#11836 = CARTESIAN_POINT ( 'NONE',  ( 10.55627441269396094, 10.31758739525044888, -223.1990319438957613 ) ) ;
#11837 = EDGE_CURVE ( 'NONE', #10545, #5175, #844, .T. ) ;
#11838 = CARTESIAN_POINT ( 'NONE',  ( -21.93223149637851677, 1.726402211042445067, -231.1052103444381203 ) ) ;
#11839 = CARTESIAN_POINT ( 'NONE',  ( 16.77642802340811556, -0.6192566135115280535, -218.8326447441449432 ) ) ;
#11840 = CARTESIAN_POINT ( 'NONE',  ( -20.69232116990083981, -0.6602618815637216754, -233.8806059993499957 ) ) ;
#11841 = CARTESIAN_POINT ( 'NONE',  ( 6.491278574642851851, 13.23281603069746382, -229.0355254242266767 ) ) ;
#11842 = CARTESIAN_POINT ( 'NONE',  ( -15.37153448429513602, 5.014568651886798456, -224.5085656291724945 ) ) ;
#11843 = CARTESIAN_POINT ( 'NONE',  ( 7.359401564398577733, 15.81697286067417707, -215.8326977948377987 ) ) ;
#11844 = CARTESIAN_POINT ( 'NONE',  ( 21.14441169763230732, 12.98245189690719315, -217.0976687089155064 ) ) ;
#11845 = CARTESIAN_POINT ( 'NONE',  ( -8.507187218596966360, -16.39771659352221533, -216.5221606441677977 ) ) ;
#11846 = EDGE_LOOP ( 'NONE', ( #19962, #7192 ) ) ;
#11847 = CARTESIAN_POINT ( 'NONE',  ( -11.55581979318669639, -19.97716813486601239, -217.5317483122086912 ) ) ;
#11848 = CARTESIAN_POINT ( 'NONE',  ( -30.17036082276531772, 5.959165309317525860, -219.4883053239162791 ) ) ;
#11849 = CARTESIAN_POINT ( 'NONE',  ( 6.374306683232226156, -13.38367253400339330, -219.9651431149896723 ) ) ;
#11850 = CARTESIAN_POINT ( 'NONE',  ( -2.817219543927646175, 14.13981714106644993, -229.6779615865167443 ) ) ;
#11851 = CARTESIAN_POINT ( 'NONE',  ( 12.32676726801020450, -8.454629307895981327, -217.7935467833756036 ) ) ;
#11852 = CARTESIAN_POINT ( 'NONE',  ( -18.34948365288241590, -1.907751280579004893, -231.5848060246952116 ) ) ;
#11853 = CARTESIAN_POINT ( 'NONE',  ( 9.125049424194871861, 12.37796447639467523, -227.2539065556229332 ) ) ;
#11854 = SURFACE_SIDE_STYLE ('',( #6901 ) ) ;
#11855 = CARTESIAN_POINT ( 'NONE',  ( -16.65220264499505376, 11.77543314451157563, -216.3149620944649030 ) ) ;
#11856 = CARTESIAN_POINT ( 'NONE',  ( 12.23475091788960434, 6.342242864926500800, -221.9572581868331156 ) ) ;
#11857 = CARTESIAN_POINT ( 'NONE',  ( 11.62313423782632782, 11.98467543564608029, -219.7293303032897995 ) ) ;
#11858 = CARTESIAN_POINT ( 'NONE',  ( 21.27834046766391651, 19.84195992785746654, -221.8454931627593965 ) ) ;
#11859 = CARTESIAN_POINT ( 'NONE',  ( -3.168869516962652622, -26.26615012824360207, -217.0152745877844040 ) ) ;
#11860 = CARTESIAN_POINT ( 'NONE',  ( -5.562203253303141359, 12.75725363875033302, -225.3078268727488478 ) ) ;
#11861 = CARTESIAN_POINT ( 'NONE',  ( 18.54610009393809023, 0.6523581019769808531, -231.1787333216317677 ) ) ;
#11862 = CARTESIAN_POINT ( 'NONE',  ( 3.247425482496454130, -26.49846316390620160, -232.4805733197358677 ) ) ;
#11863 = CARTESIAN_POINT ( 'NONE',  ( -26.19327040236159831, 13.44417515682194875, -223.7810975255189874 ) ) ;
#11864 = CARTESIAN_POINT ( 'NONE',  ( 9.880827190695510964, 24.82036951119805579, -218.1633337467656020 ) ) ;
#11865 = EDGE_CURVE ( 'NONE', #137, #9522, #10905, .T. ) ;
#11866 = CARTESIAN_POINT ( 'NONE',  ( -20.83683780809167629, -19.66850649927503625, -219.7460615899071570 ) ) ;
#11867 = CARTESIAN_POINT ( 'NONE',  ( -23.99493126334580850, 6.052326449358573335, -219.7958990219547672 ) ) ;
#11868 = CARTESIAN_POINT ( 'NONE',  ( 19.97628502126439187, 24.50819884991013708, -224.8824979922784735 ) ) ;
#11869 = ORIENTED_EDGE ( 'NONE', *, *, #11193, .F. ) ;
#11870 = CARTESIAN_POINT ( 'NONE',  ( -11.33137429837660193, 27.25022425932026238, -230.1650924901870212 ) ) ;
#11871 = CARTESIAN_POINT ( 'NONE',  ( 19.38320831645075870, -15.01455373846949293, -219.3474289024948689 ) ) ;
#11872 = CARTESIAN_POINT ( 'NONE',  ( 21.50885124049339936, -13.38680967545814404, -232.7305552638522954 ) ) ;
#11873 = LINE ( 'NONE', #4553, #12382 ) ;
#11874 = CARTESIAN_POINT ( 'NONE',  ( 4.907833106823921376, 13.98151846258800290, -229.0190609869640923 ) ) ;
#11875 = CARTESIAN_POINT ( 'NONE',  ( -23.12176686270140991, -7.251528982847554872, -234.5139663548038413 ) ) ;
#11876 = CARTESIAN_POINT ( 'NONE',  ( -8.376153411442972541, -27.59911039556260448, -219.0729038785590888 ) ) ;
#11877 = CARTESIAN_POINT ( 'NONE',  ( 11.43609017326686050, -13.06727081285745307, -217.8903327850316316 ) ) ;
#11878 = CARTESIAN_POINT ( 'NONE',  ( -8.308618357598591686, 12.44656112581930785, -228.0014162119141474 ) ) ;
#11879 = EDGE_CURVE ( 'NONE', #7196, #13305, #15977, .T. ) ;
#11880 = CARTESIAN_POINT ( 'NONE',  ( 11.05872493453861161, 12.09300746323778775, -226.7727269015348952 ) ) ;
#11881 = CARTESIAN_POINT ( 'NONE',  ( -17.39699619235753048, 15.64332637722790054, -216.0406373264262641 ) ) ;
#11882 = CARTESIAN_POINT ( 'NONE',  ( -10.46043650402819125, 8.998596506756641134, -222.4402691847174083 ) ) ;
#11883 = CARTESIAN_POINT ( 'NONE',  ( -21.81769295881711557, -14.18202798484824534, -220.2668003432649471 ) ) ;
#11884 = ORIENTED_EDGE ( 'NONE', *, *, #21643, .F. ) ;
#11885 = CARTESIAN_POINT ( 'NONE',  ( -7.965409144353247761, 13.56739834143082213, -221.6246244520798712 ) ) ;
#11886 = CARTESIAN_POINT ( 'NONE',  ( 30.52813181070726856, 5.438803974502569361, -223.5441926215666513 ) ) ;
#11887 = CARTESIAN_POINT ( 'NONE',  ( 13.32754126089433377, 12.31312334927721963, -234.6033665822900218 ) ) ;
#11888 = CARTESIAN_POINT ( 'NONE',  ( 28.81324478616323148, -9.895151559995404966, -227.1624192579662918 ) ) ;
#11889 = CARTESIAN_POINT ( 'NONE',  ( 24.63401512838761320, 0.000000000000000000, 77.51594804401857175 ) ) ;
#11890 = EDGE_LOOP ( 'NONE', ( #8187, #5568, #14308, #7561 ) ) ;
#11891 = CARTESIAN_POINT ( 'NONE',  ( -3.855805549595750392, 26.68244055262801950, -232.4569730455296508 ) ) ;
#11892 = CARTESIAN_POINT ( 'NONE',  ( -25.31373219958254595, -16.11658482301340811, -218.6250613297025609 ) ) ;
#11893 = CARTESIAN_POINT ( 'NONE',  ( 1.232595164407830946E-29, -17.50000000000007105, -60.00000000000000000 ) ) ;
#11894 = CARTESIAN_POINT ( 'NONE',  ( 14.19800769603076240, 4.587407146151301518, -224.2928935459285071 ) ) ;
#11895 = FACE_OUTER_BOUND ( 'NONE', #1343, .T. ) ;
#11896 = CARTESIAN_POINT ( 'NONE',  ( 20.38902395782249144, -18.95772103455488633, -230.9098670703349967 ) ) ;
#11897 =( NAMED_UNIT ( * ) PLANE_ANGLE_UNIT ( ) SI_UNIT ( $, .RADIAN. ) );
#11898 = CARTESIAN_POINT ( 'NONE',  ( -11.67631226053870996, 6.737291529340801333, -227.3110382950315227 ) ) ;
#11899 = CARTESIAN_POINT ( 'NONE',  ( 27.79670308438203108, 10.67628923451848877, -225.2981230784098727 ) ) ;
#11900 = CARTESIAN_POINT ( 'NONE',  ( -0.1049609700611137120, -29.11428177772140558, -224.8408750893923411 ) ) ;
#11901 = DIRECTION ( 'NONE',  ( -0.000000000000000000, -1.000000000000000000, -0.000000000000000000 ) ) ;
#11902 = CARTESIAN_POINT ( 'NONE',  ( 20.61940245508336034, -1.339931705218483815, -222.2936647182560819 ) ) ;
#11903 = DIRECTION ( 'NONE',  ( 0.000000000000000000, 0.000000000000000000, 1.000000000000000000 ) ) ;
#11904 = CARTESIAN_POINT ( 'NONE',  ( 13.43185000535467211, -22.27464880184020757, -218.9084381759842870 ) ) ;
#11905 = CARTESIAN_POINT ( 'NONE',  ( -25.95884575339096401, -1.972114683626720044, -231.2145524501483749 ) ) ;
#11906 = CARTESIAN_POINT ( 'NONE',  ( -22.62392499481471120, -4.153411067053860428, 9.102477892503269885 ) ) ;
#11907 = CARTESIAN_POINT ( 'NONE',  ( 15.20072702475037296, 19.31591084219522614, -219.7402199933931399 ) ) ;
#11908 = ADVANCED_FACE ( 'NONE', ( #14188 ), #14073, .T. ) ;
#11909 = CARTESIAN_POINT ( 'NONE',  ( 5.549682179574114471, 15.11687613544382280, -226.9959476502473308 ) ) ;
#11910 = CARTESIAN_POINT ( 'NONE',  ( 8.821624174887295666, -16.56651460208862758, -234.0193988870521196 ) ) ;
#11911 = CARTESIAN_POINT ( 'NONE',  ( 10.24538335401965661, -11.82980241027587276, -219.3753974371782363 ) ) ;
#11912 = ORIENTED_EDGE ( 'NONE', *, *, #925, .T. ) ;
#11913 = CARTESIAN_POINT ( 'NONE',  ( -7.965409144353247761, 13.56739834143082213, -221.6246244520798712 ) ) ;
#11914 = CARTESIAN_POINT ( 'NONE',  ( -19.33106196848021341, 9.919700385716687663, -219.0532654734256255 ) ) ;
#11915 = CARTESIAN_POINT ( 'NONE',  ( 12.98277799799954124, 10.30128574332056779, -221.9415428419440559 ) ) ;
#11916 = ORIENTED_EDGE ( 'NONE', *, *, #3252, .T. ) ;
#11917 = CARTESIAN_POINT ( 'NONE',  ( -7.205518813659622879, -14.37210213534873482, -226.5338589405291998 ) ) ;
#11918 = CARTESIAN_POINT ( 'NONE',  ( -0.04718088033475312248, -10.76825293233556202, 92.00000000000000000 ) ) ;
#11919 = ORIENTED_EDGE ( 'NONE', *, *, #13698, .F. ) ;
#11920 = CARTESIAN_POINT ( 'NONE',  ( 16.10828274231666768, 3.530956590605524692, -220.6574330336208050 ) ) ;
#11921 = CARTESIAN_POINT ( 'NONE',  ( 11.99204520814221553, -11.76515119196726467, -228.0494177468141572 ) ) ;
#11922 = CARTESIAN_POINT ( 'NONE',  ( 8.329997790135040603, 12.51216704542961899, -228.7022893680961602 ) ) ;
#11923 = CARTESIAN_POINT ( 'NONE',  ( -24.68906941503829700, 2.445024713909649705, -232.6803430500543755 ) ) ;
#11924 = CARTESIAN_POINT ( 'NONE',  ( 11.20713200305815427, 28.28922876448651635, -219.1239564724620834 ) ) ;
#11925 = CARTESIAN_POINT ( 'NONE',  ( -11.19223248830523332, 8.463078350427430507, -222.6400917074981578 ) ) ;
#11926 = VECTOR ( 'NONE', #8159, 1000.000000000000000 ) ;
#11927 = CARTESIAN_POINT ( 'NONE',  ( -3.843007962268670585, 27.94983497691806917, -231.4302614368887703 ) ) ;
#11928 = CARTESIAN_POINT ( 'NONE',  ( 2.476137110235832939, 10.55034688490274242, 92.00000000000001421 ) ) ;
#11929 = CARTESIAN_POINT ( 'NONE',  ( -1.890995374385051608, -13.09686096954197509, -227.5694739903412085 ) ) ;
#11930 = DIRECTION ( 'NONE',  ( 0.000000000000000000, 0.000000000000000000, 1.000000000000000000 ) ) ;
#11931 = DIRECTION ( 'NONE',  ( -0.000000000000000000, -0.000000000000000000, 1.000000000000000000 ) ) ;
#11932 = PRODUCT_DEFINITION_SHAPE ( 'NONE', 'NONE',  #110 ) ;
#11933 = CARTESIAN_POINT ( 'NONE',  ( -24.76115377241536208, -2.015397159694146456, -231.8500816169410825 ) ) ;
#11934 = CARTESIAN_POINT ( 'NONE',  ( -29.65068623107463708, 4.004319520977249525, -231.5200339834770773 ) ) ;
#11935 = CARTESIAN_POINT ( 'NONE',  ( -17.60926409178586738, -17.65542935640887023, -231.2676365506119680 ) ) ;
#11936 = CARTESIAN_POINT ( 'NONE',  ( -25.00000000000001066, 0.000000000000000000, -75.00000000000000000 ) ) ;
#11937 =( NAMED_UNIT ( * ) SI_UNIT ( $, .STERADIAN. ) SOLID_ANGLE_UNIT ( ) );
#11938 = CARTESIAN_POINT ( 'NONE',  ( 4.002939343642331949, -22.37368820207002429, -217.8631878264377804 ) ) ;
#11939 = CARTESIAN_POINT ( 'NONE',  ( 12.15450584778660570, 2.288537795953278220, -225.7049340319972828 ) ) ;
#11940 = CARTESIAN_POINT ( 'NONE',  ( -0.7041916573665241152, 14.60214745152014437, -226.3818583194645555 ) ) ;
#11941 = CARTESIAN_POINT ( 'NONE',  ( -7.694246740028670928, 10.31295298368923063, -221.9989544301487001 ) ) ;
#11942 = CARTESIAN_POINT ( 'NONE',  ( -18.99425472824626482, -3.261482901149847180, -230.2374083206451871 ) ) ;
#11943 = EDGE_LOOP ( 'NONE', ( #7256, #14821, #2185, #6040 ) ) ;
#11944 = CARTESIAN_POINT ( 'NONE',  ( 7.769483725421269860, 20.68783433326350263, -233.2348178266662728 ) ) ;
#11945 = CARTESIAN_POINT ( 'NONE',  ( -18.94444594796027914, 3.458349568010113728, -218.9807021659310635 ) ) ;
#11946 = CARTESIAN_POINT ( 'NONE',  ( -11.10182655035041144, 8.778638955377752850, -227.1050196202568827 ) ) ;
#11947 = CARTESIAN_POINT ( 'NONE',  ( -10.94940667656068634, -10.80050631132953498, -220.7362776234490127 ) ) ;
#11948 = AXIS2_PLACEMENT_3D ( 'NONE', #7659, #21698, #21365 ) ;
#11949 = DIRECTION ( 'NONE',  ( 0.000000000000000000, 0.000000000000000000, -1.000000000000000000 ) ) ;
#11950 = CARTESIAN_POINT ( 'NONE',  ( 15.37089934297015503, 20.64239674606488961, -217.2018742121147170 ) ) ;
#11951 = CARTESIAN_POINT ( 'NONE',  ( -17.30580402557236752, 11.30149179219993982, -230.8639894634705172 ) ) ;
#11952 = CARTESIAN_POINT ( 'NONE',  ( 9.169328349715531346, 20.85917603618721472, -214.7000934853629133 ) ) ;
#11953 = CARTESIAN_POINT ( 'NONE',  ( 15.18181359483165949, 6.369295616116027681, -230.7949408486033462 ) ) ;
#11954 = CIRCLE ( 'NONE', #9803, 21.50000000000001066 ) ;
#11955 = CARTESIAN_POINT ( 'NONE',  ( -8.861553082841476581, -17.08180233781500590, -216.2529452235939402 ) ) ;
#11956 = AXIS2_PLACEMENT_3D ( 'NONE', #12155, #19012, #19776 ) ;
#11957 = EDGE_LOOP ( 'NONE', ( #4452, #14287, #9568, #20145, #11690 ) ) ;
#11958 = CARTESIAN_POINT ( 'NONE',  ( -10.35216574861945560, -14.43870810227675605, -231.1876371800402126 ) ) ;
#11959 = EDGE_CURVE ( 'NONE', #566, #6745, #7430, .T. ) ;
#11960 = CARTESIAN_POINT ( 'NONE',  ( -16.23478446547628096, 26.31175924651574149, -222.4178907105033431 ) ) ;
#11961 = CARTESIAN_POINT ( 'NONE',  ( 5.982950994121768673, -14.58086824529316594, -231.1438280359330975 ) ) ;
#11962 = CARTESIAN_POINT ( 'NONE',  ( -1.249406995060579062, 25.48934319316224162, -216.9406480707515072 ) ) ;
#11963 = CARTESIAN_POINT ( 'NONE',  ( 18.64433268355766415, -12.21264687082605782, -214.8850304513305502 ) ) ;
#11964 = CARTESIAN_POINT ( 'NONE',  ( -18.53787071664277519, -6.556543064843903146, -232.5192140591401824 ) ) ;
#11965 = CARTESIAN_POINT ( 'NONE',  ( 12.47670316482120967, 2.249148913447538423, -227.4574095259895898 ) ) ;
#11966 = CARTESIAN_POINT ( 'NONE',  ( -7.770318051073092036, 21.02940971564074957, -231.8751410922876630 ) ) ;
#11967 = CARTESIAN_POINT ( 'NONE',  ( 14.29768887814754663, 10.87030385293788548, -231.8067013864770161 ) ) ;
#11968 = CARTESIAN_POINT ( 'NONE',  ( 14.54149994592679107, 8.070685273005897997, -229.7292930672863349 ) ) ;
#11969 = CARTESIAN_POINT ( 'NONE',  ( 11.75069299018312208, 6.043853022588032253, -224.2604610870103841 ) ) ;
#11970 = CARTESIAN_POINT ( 'NONE',  ( 3.668385877085885927, -11.51845067838601366, -222.7629028536941291 ) ) ;
#11971 = CARTESIAN_POINT ( 'NONE',  ( -8.985448925281199095, 11.82743561134668475, -224.1067108988273162 ) ) ;
#11972 = AXIS2_PLACEMENT_3D ( 'NONE', #9704, #13298, #18481 ) ;
#11973 = TOROIDAL_SURFACE ( 'NONE', #2958, 9.000000000000001776, 1.000000000000000000 ) ;
#11974 = CARTESIAN_POINT ( 'NONE',  ( 20.34032485158648029, 2.741617426884598530, -217.9827731991294968 ) ) ;
#11975 = CARTESIAN_POINT ( 'NONE',  ( 3.881011284096109293, -13.04786028604701187, -224.6787317506201589 ) ) ;
#11976 = CARTESIAN_POINT ( 'NONE',  ( -14.35594238341465889, 9.236863657925704629, -219.6542735655305307 ) ) ;
#11977 = CARTESIAN_POINT ( 'NONE',  ( 3.367418898937407867, 27.20023797116225595, -219.3349021808245709 ) ) ;
#11978 = CARTESIAN_POINT ( 'NONE',  ( -25.98129645912436914, -15.13773040547512139, -224.1390156429105787 ) ) ;
#11979 = CARTESIAN_POINT ( 'NONE',  ( 12.25122766587143630, 4.035812653434439845, -225.7709573147497224 ) ) ;
#11980 = CARTESIAN_POINT ( 'NONE',  ( 23.83082175545800752, 15.77842900014857896, -219.5351905769044834 ) ) ;
#11981 = VERTEX_POINT ( 'NONE', #15866 ) ;
#11982 = CARTESIAN_POINT ( 'NONE',  ( 18.23324537670537993, 23.47692953258263771, -224.8333321331434433 ) ) ;
#11983 = CARTESIAN_POINT ( 'NONE',  ( 19.92157794555808437, -7.202678279460218214, -232.3584036642729416 ) ) ;
#11984 = CARTESIAN_POINT ( 'NONE',  ( 16.26147397530412420, -13.20473954510486081, -216.9283256773164794 ) ) ;
#11985 =( NAMED_UNIT ( * ) PLANE_ANGLE_UNIT ( ) SI_UNIT ( $, .RADIAN. ) );
#11986 = CARTESIAN_POINT ( 'NONE',  ( 8.812073984913094904, 13.12649198322903210, -229.9172071780580495 ) ) ;
#11987 = CARTESIAN_POINT ( 'NONE',  ( -14.44949936980387584, -0.9990553581641278269, -220.3450678990494964 ) ) ;
#11988 = CARTESIAN_POINT ( 'NONE',  ( -2.576162127940193169, -15.57202066281789321, -231.6911579627040396 ) ) ;
#11989 = VECTOR ( 'NONE', #7207, 1000.000000000000000 ) ;
#11990 = CARTESIAN_POINT ( 'NONE',  ( 19.88636028791461641, -20.85574262981397453, -219.9907771812986823 ) ) ;
#11991 = CARTESIAN_POINT ( 'NONE',  ( -15.63515374589483109, 24.59141623553136569, -226.9057426066772507 ) ) ;
#11992 = CARTESIAN_POINT ( 'NONE',  ( 5.064106757301036765, 16.06517852189101703, -221.6413221086847329 ) ) ;
#11993 = CARTESIAN_POINT ( 'NONE',  ( -27.90314475660494153, 12.48829126175061077, -223.3300566725355338 ) ) ;
#11994 = CARTESIAN_POINT ( 'NONE',  ( -12.88152464663890306, 6.317716727793897924, -230.5294309895745073 ) ) ;
#11995 = CARTESIAN_POINT ( 'NONE',  ( 25.90657540470570197, -10.31326923046670885, -218.6707845005603019 ) ) ;
#11996 = ADVANCED_FACE ( 'NONE', ( #444 ), #14298, .F. ) ;
#11997 = ORIENTED_EDGE ( 'NONE', *, *, #17120, .T. ) ;
#11998 = CARTESIAN_POINT ( 'NONE',  ( -7.284474494690100776, 13.60812129561547046, -227.7414351104868331 ) ) ;
#11999 = CARTESIAN_POINT ( 'NONE',  ( 25.38325563848796662, 11.05100313887457553, -217.8685524735130628 ) ) ;
#12000 = CARTESIAN_POINT ( 'NONE',  ( 10.00603923119254723, 9.610873433734882454, -231.2388095806506669 ) ) ;
#12001 = CARTESIAN_POINT ( 'NONE',  ( 12.75766869239441803, -12.84633107758633663, -232.0853690516983079 ) ) ;
#12002 = FACE_OUTER_BOUND ( 'NONE', #9051, .T. ) ;
#12003 = VERTEX_POINT ( 'NONE', #7645 ) ;
#12004 = CARTESIAN_POINT ( 'NONE',  ( -3.755296588130283553, 23.77975947300719284, -233.7323173085780752 ) ) ;
#12005 = CARTESIAN_POINT ( 'NONE',  ( -8.731539701382653007, -8.828156491469059119, -227.3463890218280596 ) ) ;
#12006 = CARTESIAN_POINT ( 'NONE',  ( 0.000000000000000000, 0.000000000000000000, -60.00000000000000000 ) ) ;
#12007 = CARTESIAN_POINT ( 'NONE',  ( 14.68783945462866924, 9.535285537539673228, -219.4694094309942045 ) ) ;
#12008 = CARTESIAN_POINT ( 'NONE',  ( -14.68037037322036475, 3.441677802729143920, -220.1396515630443389 ) ) ;
#12009 = CIRCLE ( 'NONE', #2290, 2.000000000000000000 ) ;
#12010 = CARTESIAN_POINT ( 'NONE',  ( 12.02378739738799140, -16.98783239109716092, -233.4545636224233931 ) ) ;
#12011 =( NAMED_UNIT ( * ) SI_UNIT ( $, .STERADIAN. ) SOLID_ANGLE_UNIT ( ) );
#12012 = CARTESIAN_POINT ( 'NONE',  ( -11.79584727357715934, 6.509288465425584036, -222.6080315736180921 ) ) ;
#12013 = CIRCLE ( 'NONE', #6628, 2.100000000000000089 ) ;
#12014 = CARTESIAN_POINT ( 'NONE',  ( -16.15126510923403202, -0.4755054218165427615, -219.3066569788202571 ) ) ;
#12015 = CARTESIAN_POINT ( 'NONE',  ( -7.180402128846711918, -26.42159752827261698, -220.2116303544826224 ) ) ;
#12016 = DIRECTION ( 'NONE',  ( 0.000000000000000000, -1.000000000000000000, 0.000000000000000000 ) ) ;
#12017 = CARTESIAN_POINT ( 'NONE',  ( 22.00000000000000000, 2.694222958124177598E-15, -224.9999999999999716 ) ) ;
#12018 = CARTESIAN_POINT ( 'NONE',  ( -13.92046207272054303, -0.1600067567908077248, -224.5811699126800818 ) ) ;
#12019 = CARTESIAN_POINT ( 'NONE',  ( 10.81635663018848525, -11.46278932037511566, -222.6527676248099681 ) ) ;
#12020 = CARTESIAN_POINT ( 'NONE',  ( 14.06870332774840193, -1.847654110632577229, -227.3635178367878780 ) ) ;
#12021 = CARTESIAN_POINT ( 'NONE',  ( -20.96318929043787449, -9.463403270074600471, -3.248492544644434599 ) ) ;
#12022 = CARTESIAN_POINT ( 'NONE',  ( 19.59567110982616001, 18.11097967140601028, -228.7314497914969706 ) ) ;
#12023 = CARTESIAN_POINT ( 'NONE',  ( 7.497537106193371770, 19.52448593130572618, -231.1338690134634248 ) ) ;
#12024 = CARTESIAN_POINT ( 'NONE',  ( 20.22673842361927399, -24.21895433676095877, -222.6595898022596316 ) ) ;
#12025 = CARTESIAN_POINT ( 'NONE',  ( 7.021536848793814123, -14.49751826649810482, -218.4909385705359455 ) ) ;
#12026 = ORIENTED_EDGE ( 'NONE', *, *, #4848, .F. ) ;
#12027 = CARTESIAN_POINT ( 'NONE',  ( -10.40174557315337900, 22.75579539577861965, -231.4492192189165962 ) ) ;
#12028 = CARTESIAN_POINT ( 'NONE',  ( -18.33565906012873725, 9.491905303418088025, -219.1855745749628568 ) ) ;
#12029 = CARTESIAN_POINT ( 'NONE',  ( -13.34869474643618581, 6.516017165032126357, -231.2228057326931321 ) ) ;
#12030 = CIRCLE ( 'NONE', #7376, 5.000000000000000888 ) ;
#12031 = CARTESIAN_POINT ( 'NONE',  ( -14.13544422886439911, -23.73189729233824252, -223.0800202563271171 ) ) ;
#12032 = CARTESIAN_POINT ( 'NONE',  ( -10.75822951548915185, -1.509788170712045297, 92.00000000000002842 ) ) ;
#12033 = ORIENTED_EDGE ( 'NONE', *, *, #7496, .F. ) ;
#12034 = CARTESIAN_POINT ( 'NONE',  ( 13.14260364752544596, 5.866423290307341887, -222.7705901084601408 ) ) ;
#12035 = CARTESIAN_POINT ( 'NONE',  ( 17.04113992636424513, -19.77713422747145700, -220.8032168804961373 ) ) ;
#12036 = CARTESIAN_POINT ( 'NONE',  ( 10.50530447320976535, 20.19629329636330084, -217.1354359361034767 ) ) ;
#12037 = CARTESIAN_POINT ( 'NONE',  ( -7.189383125363055349, 14.28512618638020548, -231.7475838278701303 ) ) ;
#12038 = EDGE_CURVE ( 'NONE', #722, #9014, #7688, .T. ) ;
#12039 = CARTESIAN_POINT ( 'NONE',  ( 18.59615491886314231, -0.2392802120807639710, -217.5848846836084078 ) ) ;
#12040 = ADVANCED_FACE ( 'NONE', ( #6275 ), #12926, .F. ) ;
#12041 = CARTESIAN_POINT ( 'NONE',  ( -8.172572110426221670, 16.86653848210977813, -233.4220330256369493 ) ) ;
#12042 = CIRCLE ( 'NONE', #3774, 22.92944763917984474 ) ;
#12043 = CARTESIAN_POINT ( 'NONE',  ( 15.52719855059926424, 1.633696074270991172, -221.7349885876216433 ) ) ;
#12044 = CARTESIAN_POINT ( 'NONE',  ( 8.532614294830283441, -28.73326933124977955, -229.1610356131385231 ) ) ;
#12045 = PRESENTATION_LAYER_ASSIGNMENT (  '', '', ( #22095 ) ) ;
#12046 = CARTESIAN_POINT ( 'NONE',  ( 22.03647168421188240, 0.3315607655626218175, -232.0572713672587213 ) ) ;
#12047 = DIRECTION ( 'NONE',  ( 1.000000000000000000, 0.000000000000000000, 0.000000000000000000 ) ) ;
#12048 = CARTESIAN_POINT ( 'NONE',  ( -26.07210576407111446, -8.413030596423759278, -230.6002792590230115 ) ) ;
#12049 = CARTESIAN_POINT ( 'NONE',  ( 18.54610009393809023, 0.6523581019769808531, -231.1787333216317677 ) ) ;
#12050 = CARTESIAN_POINT ( 'NONE',  ( -14.91191843134457784, -11.59770670008449756, -219.5316993567479642 ) ) ;
#12051 = CARTESIAN_POINT ( 'NONE',  ( 7.092430827040528740, -27.48041265710635628, -228.4891580147104548 ) ) ;
#12052 = CARTESIAN_POINT ( 'NONE',  ( 17.41909632439413969, 2.006477695503792624, -233.4081875040758121 ) ) ;
#12053 = CARTESIAN_POINT ( 'NONE',  ( 9.336393807558161839, 27.79372469574263960, -228.5913636680961361 ) ) ;
#12054 = CARTESIAN_POINT ( 'NONE',  ( -20.38637754046084183, 19.95723714148678241, -217.5201383746364172 ) ) ;
#12055 = ORIENTED_EDGE ( 'NONE', *, *, #20398, .T. ) ;
#12056 = CARTESIAN_POINT ( 'NONE',  ( 30.90240445905660138, -9.617167762261830788, -225.5262352394493064 ) ) ;
#12057 = ORIENTED_EDGE ( 'NONE', *, *, #19702, .T. ) ;
#12058 = CARTESIAN_POINT ( 'NONE',  ( 13.43170911749896490, 19.07691563292472026, -232.7497845103644636 ) ) ;
#12059 = CARTESIAN_POINT ( 'NONE',  ( -14.58084844870496966, 13.85720943031455832, -233.3219724312919254 ) ) ;
#12060 = CARTESIAN_POINT ( 'NONE',  ( -22.70558257617108922, 14.65737936663030538, -230.9775454010380997 ) ) ;
#12061 = CARTESIAN_POINT ( 'NONE',  ( -16.87231408860552051, -20.68405295654727993, -231.0270656955280515 ) ) ;
#12062 = VECTOR ( 'NONE', #10357, 1000.000000000000000 ) ;
#12063 =( GEOMETRIC_REPRESENTATION_CONTEXT ( 3 ) GLOBAL_UNCERTAINTY_ASSIGNED_CONTEXT ( ( #21791 ) ) GLOBAL_UNIT_ASSIGNED_CONTEXT ( ( #11184, #7923, #19722 ) ) REPRESENTATION_CONTEXT ( 'NONE', 'WORKASPACE' ) );
#12064 = DIRECTION ( 'NONE',  ( -0.000000000000000000, -0.000000000000000000, 1.000000000000000000 ) ) ;
#12065 = CYLINDRICAL_SURFACE ( 'NONE', #9928, 23.00000000000000000 ) ;
#12066 = CARTESIAN_POINT ( 'NONE',  ( -20.29166677327761903, 16.18344358422343632, -220.0060062064338524 ) ) ;
#12067 = CARTESIAN_POINT ( 'NONE',  ( 10.02118533929671074, 10.65166262057242008, -217.7534731326719566 ) ) ;
#12068 = CARTESIAN_POINT ( 'NONE',  ( 12.56362091610784049, 9.747446748398973071, -231.6428467497164547 ) ) ;
#12069 = CARTESIAN_POINT ( 'NONE',  ( -16.68014207497104451, -3.425858445063780788, -215.9332308579483595 ) ) ;
#12070 = ORIENTED_EDGE ( 'NONE', *, *, #4685, .F. ) ;
#12071 = CARTESIAN_POINT ( 'NONE',  ( -5.056986327342952947, -15.36481113542577503, -220.7955371552936583 ) ) ;
#12072 = CARTESIAN_POINT ( 'NONE',  ( -8.894613172508529786, 25.42460746921206294, -232.3150764041658363 ) ) ;
#12073 = CARTESIAN_POINT ( 'NONE',  ( 11.14834367153813233, -21.42845646353120870, -216.4520112529555718 ) ) ;
#12074 = CARTESIAN_POINT ( 'NONE',  ( -6.571166997218196748, 12.74865329367398736, -229.9840124400968762 ) ) ;
#12075 = CARTESIAN_POINT ( 'NONE',  ( 24.71064586368820315, -12.65488197590634378, -232.9862317762581654 ) ) ;
#12076 =( GEOMETRIC_REPRESENTATION_CONTEXT ( 3 ) GLOBAL_UNCERTAINTY_ASSIGNED_CONTEXT ( ( #19550 ) ) GLOBAL_UNIT_ASSIGNED_CONTEXT ( ( #7619, #10997, #14050 ) ) REPRESENTATION_CONTEXT ( 'NONE', 'WORKASPACE' ) );
#12077 = CARTESIAN_POINT ( 'NONE',  ( -25.10035252441274167, -15.33546242866430198, -228.3913311683031964 ) ) ;
#12078 = CARTESIAN_POINT ( 'NONE',  ( -15.83178333309709629, 2.467763724635483324, -230.4064772870105458 ) ) ;
#12079 = PLANE ( 'NONE',  #20689 ) ;
#12080 = CARTESIAN_POINT ( 'NONE',  ( -1.364406401035816785, 24.33111505239456918, -219.5658712396381418 ) ) ;
#12081 = CARTESIAN_POINT ( 'NONE',  ( -14.06164063153489252, 2.050767714179807744, -227.2881998904968270 ) ) ;
#12082 = CARTESIAN_POINT ( 'NONE',  ( 15.89706143421296147, 10.57416387607782227, -218.3862415393350318 ) ) ;
#12083 = CARTESIAN_POINT ( 'NONE',  ( 21.17011458613547248, 1.652544727609948527, -234.6098499860487152 ) ) ;
#12084 = CARTESIAN_POINT ( 'NONE',  ( 5.535251771770903773, -29.91249465213552128, -219.7039649384792028 ) ) ;
#12085 = CARTESIAN_POINT ( 'NONE',  ( 13.79814099039094089, 16.09927043668092850, -214.6489469124405502 ) ) ;
#12086 = DIRECTION ( 'NONE',  ( -1.000000000000000000, 0.000000000000000000, 0.000000000000000000 ) ) ;
#12087 = CARTESIAN_POINT ( 'NONE',  ( -6.776294192501696401, -30.39940938379458046, -221.2799938066956997 ) ) ;
#12088 = CARTESIAN_POINT ( 'NONE',  ( -10.30870167223346456, 11.95603877111467561, -228.4123369090513336 ) ) ;
#12089 = AXIS2_PLACEMENT_3D ( 'NONE', #20550, #5249, #22145 ) ;
#12090 = CARTESIAN_POINT ( 'NONE',  ( 2.893760225568064115, 14.39521026618305477, -227.6654023557511550 ) ) ;
#12091 = CARTESIAN_POINT ( 'NONE',  ( -20.76924187596804217, -21.50248317380421170, -228.3679492147379335 ) ) ;
#12092 = CARTESIAN_POINT ( 'NONE',  ( -22.90687623753526125, 9.466200233939549236, -230.1557007022273638 ) ) ;
#12093 = CARTESIAN_POINT ( 'NONE',  ( 25.02650711521362936, 17.58144575069911042, -223.6165279156031431 ) ) ;
#12094 = ORIENTED_EDGE ( 'NONE', *, *, #550, .T. ) ;
#12095 = CARTESIAN_POINT ( 'NONE',  ( 17.97843143658897347, 22.12221935793617078, -220.9346589834416079 ) ) ;
#12096 = CARTESIAN_POINT ( 'NONE',  ( 17.78250599636351481, -9.160802950715318360, -218.6762383290621869 ) ) ;
#12097 = ORIENTED_EDGE ( 'NONE', *, *, #17705, .T. ) ;
#12098 = CARTESIAN_POINT ( 'NONE',  ( 27.81506808824343580, -10.52944849582878106, -221.0913368219556503 ) ) ;
#12099 = FILL_AREA_STYLE_COLOUR ( '', #12749 ) ;
#12100 = CARTESIAN_POINT ( 'NONE',  ( 19.72515656911863147, 14.02277373989196541, -218.0718040828188009 ) ) ;
#12101 = CARTESIAN_POINT ( 'NONE',  ( -14.05955845762884238, -0.8719634938775207011, -221.0475910153949428 ) ) ;
#12102 = CARTESIAN_POINT ( 'NONE',  ( -6.163092920833200594, -27.00835405423771007, -232.1022292408408987 ) ) ;
#12103 = CARTESIAN_POINT ( 'NONE',  ( 21.05631363308661363, -21.50266115212419393, -222.6654548186096747 ) ) ;
#12104 = CARTESIAN_POINT ( 'NONE',  ( 1.455106383990497187, 21.12056149333958999, -230.8076663600630241 ) ) ;
#12105 = DIRECTION ( 'NONE',  ( 0.000000000000000000, 0.000000000000000000, 1.000000000000000000 ) ) ;
#12106 = CARTESIAN_POINT ( 'NONE',  ( 15.08139719848974103, 12.15862464477973504, -219.3112749338812080 ) ) ;
#12107 = CARTESIAN_POINT ( 'NONE',  ( -10.65455960636934662, 10.37188583052882862, -219.5197110153079620 ) ) ;
#12108 = CARTESIAN_POINT ( 'NONE',  ( -6.769588938507062004, 18.22485903270490937, -231.3660928915624879 ) ) ;
#12109 = CARTESIAN_POINT ( 'NONE',  ( 28.46281617689634302, -10.50803404096709137, -222.5507679334694728 ) ) ;
#12110 = CARTESIAN_POINT ( 'NONE',  ( 3.160467108836292116, 14.95099014189016629, -228.9242958482614370 ) ) ;
#12111 = CARTESIAN_POINT ( 'NONE',  ( 13.16746181015946959, 0.3897807143096829741, -227.1676274388083243 ) ) ;
#12112 = CARTESIAN_POINT ( 'NONE',  ( 11.38520239593705163, 18.87760105923376486, -235.3435298574111130 ) ) ;
#12113 = CARTESIAN_POINT ( 'NONE',  ( 13.07616324839670341, -23.69356132834180784, -230.7206382488779184 ) ) ;
#12114 = CARTESIAN_POINT ( 'NONE',  ( 26.00000000000000000, -0.5000000000000000000, -6.000000000000000000 ) ) ;
#12115 = ORIENTED_EDGE ( 'NONE', *, *, #21236, .F. ) ;
#12116 = CARTESIAN_POINT ( 'NONE',  ( -7.395406416482832590, 12.93623984139929739, -219.2606224730616873 ) ) ;
#12117 = CARTESIAN_POINT ( 'NONE',  ( -22.42461747750134293, -16.81348984091923171, -233.1118345967658172 ) ) ;
#12118 = DIRECTION ( 'NONE',  ( 0.000000000000000000, 0.000000000000000000, 1.000000000000000000 ) ) ;
#12119 = CARTESIAN_POINT ( 'NONE',  ( 21.39553407250273054, 8.453402029343234148, -217.9531594780983141 ) ) ;
#12120 = CARTESIAN_POINT ( 'NONE',  ( -16.20072894238734307, 0.5024448614660336210, -230.4554067149722130 ) ) ;
#12121 = CARTESIAN_POINT ( 'NONE',  ( 18.55298002304457228, -12.22359628793950570, -216.9137843736221782 ) ) ;
#12122 = CARTESIAN_POINT ( 'NONE',  ( -15.82069055112642353, 8.315535108674763976, -217.2800172218543935 ) ) ;
#12123 = CARTESIAN_POINT ( 'NONE',  ( -20.43618815875133521, 1.403378831510147196, -232.9646741665398224 ) ) ;
#12124 = EDGE_CURVE ( 'NONE', #8392, #20174, #994, .T. ) ;
#12125 = CARTESIAN_POINT ( 'NONE',  ( -1.380908993000753648, -20.21092959135559752, -218.0995018783601438 ) ) ;
#12126 = DIRECTION ( 'NONE',  ( -1.000000000000000000, 0.000000000000000000, 0.000000000000000000 ) ) ;
#12127 = CARTESIAN_POINT ( 'NONE',  ( -21.12229863832016008, 9.103146205856329942, 4.151976327957419777 ) ) ;
#12128 = CARTESIAN_POINT ( 'NONE',  ( -22.11084984981285118, 10.96048252433489623, -216.6117774006995376 ) ) ;
#12129 = CARTESIAN_POINT ( 'NONE',  ( 15.76600796393256410, -24.40864267010898558, -225.5036181134576907 ) ) ;
#12130 = CARTESIAN_POINT ( 'NONE',  ( 13.36754297251702717, -1.844478585726079256, -222.6328387543338181 ) ) ;
#12131 = CARTESIAN_POINT ( 'NONE',  ( -24.49077085807447318, 5.028751554214830222, 8.649788737574644060 ) ) ;
#12132 = CARTESIAN_POINT ( 'NONE',  ( 20.92326490933994876, 18.00580109995737033, -222.6060933800056034 ) ) ;
#12133 = CARTESIAN_POINT ( 'NONE',  ( -10.98447002683091256, 8.146786682930290624, -230.8316952156193338 ) ) ;
#12134 = CARTESIAN_POINT ( 'NONE',  ( 13.96918721733258195, 14.12724320058294403, -230.4946432816737172 ) ) ;
#12135 = CARTESIAN_POINT ( 'NONE',  ( -1.494569538902034145, -28.29191435206508487, -228.8702894339512852 ) ) ;
#12136 = CARTESIAN_POINT ( 'NONE',  ( 30.29962988386644085, -7.724198041227372080, -225.2151988352147782 ) ) ;
#12137 = VERTEX_POINT ( 'NONE', #7869 ) ;
#12138 = CARTESIAN_POINT ( 'NONE',  ( -16.07193224038526580, 12.24477688577882439, -232.1409653212175499 ) ) ;
#12139 = CARTESIAN_POINT ( 'NONE',  ( -23.52458685063474420, 4.195399146287285497, -230.7490123595086970 ) ) ;
#12140 = CARTESIAN_POINT ( 'NONE',  ( -17.17981675979428147, 1.478343374046288128, -216.2419730925687418 ) ) ;
#12141 = CARTESIAN_POINT ( 'NONE',  ( -4.572289063834428013, -16.67516242687949557, -229.9678395161569142 ) ) ;
#12142 = DIRECTION ( 'NONE',  ( -1.083936797661037871E-15, -1.000000000000000000, 0.000000000000000000 ) ) ;
#12143 = ORIENTED_EDGE ( 'NONE', *, *, #10113, .T. ) ;
#12144 = CARTESIAN_POINT ( 'NONE',  ( 22.42095341476093040, 9.457779162868732215, -232.6339572190428555 ) ) ;
#12145 = CARTESIAN_POINT ( 'NONE',  ( 11.63667859525082093, -10.90089931597979600, -224.9413544669828013 ) ) ;
#12146 = CARTESIAN_POINT ( 'NONE',  ( 3.763426558366607111, 28.60172112197566818, -230.1816715025297526 ) ) ;
#12147 = CARTESIAN_POINT ( 'NONE',  ( -8.172572110426221670, 16.86653848210977813, -233.4220330256369493 ) ) ;
#12148 = CARTESIAN_POINT ( 'NONE',  ( 13.21888801141564151, 2.135177519634172238, -228.0426311217386797 ) ) ;
#12149 = EDGE_CURVE ( 'NONE', #16621, #16938, #16312, .T. ) ;
#12150 = CARTESIAN_POINT ( 'NONE',  ( 8.496844655769807630, 14.66037471857024599, -219.1631158796573118 ) ) ;
#12151 = FACE_OUTER_BOUND ( 'NONE', #20261, .T. ) ;
#12152 = CARTESIAN_POINT ( 'NONE',  ( -7.460068573003235670, -29.58770008691625364, -228.1902472473001637 ) ) ;
#12153 = CARTESIAN_POINT ( 'NONE',  ( 18.00123703865980218, -15.82960056198189491, -233.0014896689109776 ) ) ;
#12154 = PLANE ( 'NONE',  #19939 ) ;
#12155 = CARTESIAN_POINT ( 'NONE',  ( 0.000000000000000000, 0.000000000000000000, -75.00000000000000000 ) ) ;
#12156 = CARTESIAN_POINT ( 'NONE',  ( -9.924247690135956645, 7.079756654796299564, -222.1205998075789694 ) ) ;
#12157 = CARTESIAN_POINT ( 'NONE',  ( -17.33275459786259276, -4.423804729537573088, -220.8440611986277418 ) ) ;
#12158 = ADVANCED_FACE ( 'NONE', ( #21348 ), #14179, .F. ) ;
#12159 = CARTESIAN_POINT ( 'NONE',  ( 14.19979467405507556, 6.351366891014061267, -230.8614099669030679 ) ) ;
#12160 = CARTESIAN_POINT ( 'NONE',  ( 3.192353461299334061, 22.13718518159985393, -217.1103300728619843 ) ) ;
#12161 = CARTESIAN_POINT ( 'NONE',  ( 3.100794261777709782, 20.70580715608724276, -231.8781843337728219 ) ) ;
#12162 = ORIENTED_EDGE ( 'NONE', *, *, #17409, .T. ) ;
#12163 = CARTESIAN_POINT ( 'NONE',  ( -27.92538795710911259, -2.661554249663629079, -224.6264721727631581 ) ) ;
#12164 = CARTESIAN_POINT ( 'NONE',  ( 16.54345861550681107, 19.37554510112122230, -218.2240151908141002 ) ) ;
#12165 = CARTESIAN_POINT ( 'NONE',  ( -8.329232059016652201, 11.81357365351366617, -230.1839637212758021 ) ) ;
#12166 = CARTESIAN_POINT ( 'NONE',  ( -13.43384090552117271, 6.057765724406720231, -225.7182623230366119 ) ) ;
#12167 = CARTESIAN_POINT ( 'NONE',  ( -19.18273340400098448, -14.85130345181434741, -232.7114379411565039 ) ) ;
#12168 = CARTESIAN_POINT ( 'NONE',  ( -15.15434969228324924, 4.423874646950748613, -230.6144467931089821 ) ) ;
#12169 = VECTOR ( 'NONE', #20424, 1000.000000000000000 ) ;
#12170 = CARTESIAN_POINT ( 'NONE',  ( 0.000000000000000000, 0.000000000000000000, -78.50000000000000000 ) ) ;
#12171 = CARTESIAN_POINT ( 'NONE',  ( -10.76794919243112325, 1.318693451189210089E-15, 92.50000000000000000 ) ) ;
#12172 = CARTESIAN_POINT ( 'NONE',  ( 17.91327661571172314, 1.545939370248587075, -216.9938266089438912 ) ) ;
#12173 = CARTESIAN_POINT ( 'NONE',  ( -10.45265333418718612, 16.71118685480038479, -231.7490466715443631 ) ) ;
#12174 = CLOSED_SHELL ( 'NONE', ( #5545, #3538, #9983, #14561, #1820, #21092, #9260, #8449, #5016, #11908, #21845, #3186, #12520, #7335, #20015, #6180, #1393, #16205, #4576 ) ) ;
#12175 = CARTESIAN_POINT ( 'NONE',  ( 11.50837930502119733, 10.86662242793286381, -233.1728506169798436 ) ) ;
#12176 = CARTESIAN_POINT ( 'NONE',  ( 20.88210880980788531, 0.9259446317980322139, -218.6312544800709929 ) ) ;
#12177 = CARTESIAN_POINT ( 'NONE',  ( -22.42461747750134293, -16.81348984091923171, -233.1118345967658172 ) ) ;
#12178 = CARTESIAN_POINT ( 'NONE',  ( -28.74911369566071784, -10.37195270599671737, -225.4617258471509729 ) ) ;
#12179 = CIRCLE ( 'NONE', #7518, 19.63401512838747820 ) ;
#12180 = CARTESIAN_POINT ( 'NONE',  ( -13.58389614404818069, 15.11490620317918676, -215.3922994348461941 ) ) ;
#12181 = CARTESIAN_POINT ( 'NONE',  ( 0.04660897052267574947, -31.13860575300111577, -224.7746869833732717 ) ) ;
#12182 = CARTESIAN_POINT ( 'NONE',  ( -3.368164009525018265, 19.03203264544105622, -233.5986411977714567 ) ) ;
#12183 = CARTESIAN_POINT ( 'NONE',  ( 27.24384134789437439, -15.00887433271272364, -228.9543321217944083 ) ) ;
#12184 = CARTESIAN_POINT ( 'NONE',  ( 13.80743592543072396, -3.637675435010108906E-12, -228.0000000000000568 ) ) ;
#12185 = CARTESIAN_POINT ( 'NONE',  ( 18.30177952310522471, 1.918278963380847468, -233.8574151782075887 ) ) ;
#12186 = DIRECTION ( 'NONE',  ( -1.000000000000000000, 0.000000000000000000, 0.000000000000000000 ) ) ;
#12187 = CARTESIAN_POINT ( 'NONE',  ( 0.04449911090679885967, 16.51968908208873899, -222.9067194156212111 ) ) ;
#12188 = CARTESIAN_POINT ( 'NONE',  ( -21.28183200535960040, 1.085030287403131233, -217.0000000015322712 ) ) ;
#12189 = CARTESIAN_POINT ( 'NONE',  ( 18.60971343765040942, 2.368090295052050820, -218.6871071987073094 ) ) ;
#12190 = CARTESIAN_POINT ( 'NONE',  ( 13.25330606581809789, 10.40242132629824034, -230.9170765704288044 ) ) ;
#12191 = CARTESIAN_POINT ( 'NONE',  ( -2.619247311076123630, -29.90652300472198988, -220.3405913430138128 ) ) ;
#12192 = CARTESIAN_POINT ( 'NONE',  ( 7.283976506941576723, 24.82246917020504284, -234.3244871078919402 ) ) ;
#12193 = DIRECTION ( 'NONE',  ( 0.000000000000000000, 0.000000000000000000, -1.000000000000000000 ) ) ;
#12194 = CARTESIAN_POINT ( 'NONE',  ( -3.739406429132753562, -13.42303118918103344, -219.1969888661882635 ) ) ;
#12195 = CARTESIAN_POINT ( 'NONE',  ( -17.14223598032838325, 23.31797360549976261, -226.5771676936548431 ) ) ;
#12196 = CARTESIAN_POINT ( 'NONE',  ( 16.64575860537911112, 25.12688477742292648, -227.5050599151411745 ) ) ;
#12197 = CARTESIAN_POINT ( 'NONE',  ( -22.20848920810297855, -2.028924892417935055, -232.4401719831211039 ) ) ;
#12198 = CARTESIAN_POINT ( 'NONE',  ( -18.42638600874552424, 7.060399206045774534, -230.3991437614443214 ) ) ;
#12199 = CARTESIAN_POINT ( 'NONE',  ( -12.26337789213896201, 9.274758280606999250, -219.9806108963443876 ) ) ;
#12200 = CARTESIAN_POINT ( 'NONE',  ( 17.66865342763861690, 2.849170916951684784, -230.9175656266857004 ) ) ;
#12201 = VERTEX_POINT ( 'NONE', #19995 ) ;
#12202 = CARTESIAN_POINT ( 'NONE',  ( 10.78187269046063435, 10.73871010366167944, -221.9206544238666368 ) ) ;
#12203 = CARTESIAN_POINT ( 'NONE',  ( 13.77063830053042892, -24.19668776886549821, -225.6207953771408086 ) ) ;
#12204 = ORIENTED_EDGE ( 'NONE', *, *, #4766, .T. ) ;
#12205 = CARTESIAN_POINT ( 'NONE',  ( 13.39541376241636783, -3.462025909069690321, -228.4300562622815391 ) ) ;
#12206 = CARTESIAN_POINT ( 'NONE',  ( 1.296323513242173542, 20.09034598902932345, -230.5712631353794961 ) ) ;
#12207 = EDGE_LOOP ( 'NONE', ( #17976, #12661, #3676, #3299 ) ) ;
#12208 = CARTESIAN_POINT ( 'NONE',  ( 0.000000000000000000, 23.00000000000000000, 69.99999999999998579 ) ) ;
#12209 = CARTESIAN_POINT ( 'NONE',  ( 8.689059922489732912, 15.18271246186214363, -218.7354841152034908 ) ) ;
#12210 = CARTESIAN_POINT ( 'NONE',  ( -14.30218759248275084, -10.01744029472290620, -234.2423117832250341 ) ) ;
#12211 = CARTESIAN_POINT ( 'NONE',  ( -5.804961988600464196, -12.67915086496026511, -228.7923277404792088 ) ) ;
#12212 = CARTESIAN_POINT ( 'NONE',  ( 1.541778504653760429, -23.48174737203985529, -233.9922866444541967 ) ) ;
#12213 = CARTESIAN_POINT ( 'NONE',  ( -9.060146982536336324, 27.14942986116457746, -225.6568961786626062 ) ) ;
#12214 = DIRECTION ( 'NONE',  ( 1.000000000000000000, 0.000000000000000000, 0.000000000000000000 ) ) ;
#12215 = CARTESIAN_POINT ( 'NONE',  ( 20.92326490933994876, 18.00580109995737033, -222.6060933800056034 ) ) ;
#12216 = EDGE_CURVE ( 'NONE', #7787, #10628, #5942, .T. ) ;
#12217 = CARTESIAN_POINT ( 'NONE',  ( -13.65925618638770800, 3.289586759644148817, -222.1579143493116533 ) ) ;
#12218 = CARTESIAN_POINT ( 'NONE',  ( -9.403561938624596550, 12.70246821120386471, -220.7484614495429582 ) ) ;
#12219 = CARTESIAN_POINT ( 'NONE',  ( 9.527502190795640757, 23.55559004943647139, -217.4101659741468211 ) ) ;
#12220 = CARTESIAN_POINT ( 'NONE',  ( 18.40125535140034430, 0.01434342441762339639, -233.2485400239426099 ) ) ;
#12221 = CARTESIAN_POINT ( 'NONE',  ( 13.34963947135311102, 7.416462695144936390, -217.9359469527792044 ) ) ;
#12222 = CARTESIAN_POINT ( 'NONE',  ( 7.739744183733028748, -12.54214339878522999, -227.5419174737939159 ) ) ;
#12223 = CARTESIAN_POINT ( 'NONE',  ( -1.232595164407830946E-29, 17.50000000000007105, -24.99999999999999645 ) ) ;
#12224 = ORIENTED_EDGE ( 'NONE', *, *, #21373, .F. ) ;
#12225 = CARTESIAN_POINT ( 'NONE',  ( -2.808235066048971440, 30.42019778760651150, -222.6481917607299295 ) ) ;
#12226 = CARTESIAN_POINT ( 'NONE',  ( 22.78751929883380356, -1.647884454956899836, -231.3901500139513416 ) ) ;
#12227 = CARTESIAN_POINT ( 'NONE',  ( 24.21331552874348958, 0.07051084380047288602, -231.7986140076958463 ) ) ;
#12228 = CARTESIAN_POINT ( 'NONE',  ( 15.42212722119060864, 5.401662248084913465, -220.8333402320903645 ) ) ;
#12229 = CARTESIAN_POINT ( 'NONE',  ( -28.17543631911187063, 3.557555778861649642, -230.1980773687482156 ) ) ;
#12230 = CARTESIAN_POINT ( 'NONE',  ( 5.434900225474387447, -11.93567727083262042, -224.7511004068755369 ) ) ;
#12231 = DIRECTION ( 'NONE',  ( 1.000000000000000000, 0.000000000000000000, 0.000000000000000000 ) ) ;
#12232 = CARTESIAN_POINT ( 'NONE',  ( -7.913358619554302642, 16.16796202616373890, -233.0981776325470491 ) ) ;
#12233 = ORIENTED_EDGE ( 'NONE', *, *, #21602, .F. ) ;
#12234 = CARTESIAN_POINT ( 'NONE',  ( -13.10651848559790444, 3.262242204071156948, -224.3513854875720597 ) ) ;
#12235 = CARTESIAN_POINT ( 'NONE',  ( -18.96646980336054611, -22.16549408654085696, -227.7928771762007329 ) ) ;
#12236 = CARTESIAN_POINT ( 'NONE',  ( -2.465190328815661892E-29, -25.00000000000012790, -75.00000000000000000 ) ) ;
#12237 = CARTESIAN_POINT ( 'NONE',  ( -22.99291885829180515, 0.6598326085037610200, 9.983746764812034158 ) ) ;
#12238 = CARTESIAN_POINT ( 'NONE',  ( -26.58771759052039485, 5.114955214121561511, -218.2823714869195442 ) ) ;
#12239 = CARTESIAN_POINT ( 'NONE',  ( 13.24102317311734112, -10.11186274821533715, -227.6843928184991057 ) ) ;
#12240 = CARTESIAN_POINT ( 'NONE',  ( -22.20848920810297855, -2.028924892417935055, -232.4401719831211039 ) ) ;
#12241 = CARTESIAN_POINT ( 'NONE',  ( -22.91284222278097360, 10.00008306376378364, -0.6577592246564750722 ) ) ;
#12242 = EDGE_CURVE ( 'NONE', #7196, #3873, #12820, .T. ) ;
#12243 = CARTESIAN_POINT ( 'NONE',  ( 20.59763700141659015, 7.383112456150029423, -232.0722244125682039 ) ) ;
#12244 = CARTESIAN_POINT ( 'NONE',  ( -7.694246740028670928, 10.31295298368923063, -221.9989544301487001 ) ) ;
#12245 = CARTESIAN_POINT ( 'NONE',  ( 24.93482953594869755, 13.13888391581411241, -222.4369546851285691 ) ) ;
#12246 = CARTESIAN_POINT ( 'NONE',  ( -0.7782973328492528431, -21.73504563028646075, -232.5926793935175283 ) ) ;
#12247 = CARTESIAN_POINT ( 'NONE',  ( 17.72923050078999907, -1.936365952008033853, -232.4832991314195567 ) ) ;
#12248 = EDGE_LOOP ( 'NONE', ( #7627, #2722, #21380, #17017 ) ) ;
#12249 = CARTESIAN_POINT ( 'NONE',  ( 2.485733319737138736, 14.76073968410796056, -221.5245536174130905 ) ) ;
#12250 = CARTESIAN_POINT ( 'NONE',  ( -14.01525440049806193, 8.239250543314939890, -226.5804714421811070 ) ) ;
#12251 = CARTESIAN_POINT ( 'NONE',  ( 22.24262848503957812, 2.205713500382371794, -232.7243927205662430 ) ) ;
#12252 = CARTESIAN_POINT ( 'NONE',  ( -23.09090074015852778, -15.52172445179926896, -222.9863534629544972 ) ) ;
#12253 = DIRECTION ( 'NONE',  ( 0.000000000000000000, -1.000000000000000000, 0.000000000000000000 ) ) ;
#12254 = VERTEX_POINT ( 'NONE', #19663 ) ;
#12255 = CARTESIAN_POINT ( 'NONE',  ( 26.53121369294028042, 10.74560293343441586, -229.2288136770759195 ) ) ;
#12256 = CARTESIAN_POINT ( 'NONE',  ( 3.050495372378628112, -23.18092737088175781, -231.5841725462776992 ) ) ;
#12257 = CARTESIAN_POINT ( 'NONE',  ( 12.99034161053428349, 11.71468708507361889, -230.9043293568357740 ) ) ;
#12258 = CARTESIAN_POINT ( 'NONE',  ( -10.45786516112131892, 23.61456281964591852, -233.2869923610001592 ) ) ;
#12259 = CARTESIAN_POINT ( 'NONE',  ( 11.21112214669106777, 5.418350954422431975, -227.6539796508718325 ) ) ;
#12260 = CARTESIAN_POINT ( 'NONE',  ( 4.730976410881341465, 17.65764351829336931, -217.6025626048331674 ) ) ;
#12261 = CARTESIAN_POINT ( 'NONE',  ( 0.000000000000000000, 0.000000000000000000, -69.99999999999998579 ) ) ;
#12262 = CARTESIAN_POINT ( 'NONE',  ( 1.623338700557370951, -21.82196275546919040, -234.1129525514646730 ) ) ;
#12263 = CARTESIAN_POINT ( 'NONE',  ( 19.88636028791461641, -20.85574262981397453, -219.9907771812986823 ) ) ;
#12264 = CARTESIAN_POINT ( 'NONE',  ( 25.50000000000000000, -0.5000000000000000000, 0.000000000000000000 ) ) ;
#12265 = CARTESIAN_POINT ( 'NONE',  ( 0.000000000000000000, 0.000000000000000000, 93.00000000000000000 ) ) ;
#12266 = CARTESIAN_POINT ( 'NONE',  ( -12.61443312487471324, 8.399394471292156439, -217.5740162615319093 ) ) ;
#12267 = CARTESIAN_POINT ( 'NONE',  ( -26.25663555152313222, -8.728475094464092976, -226.4697227271102236 ) ) ;
#12268 = CARTESIAN_POINT ( 'NONE',  ( -14.58575946311604277, 2.190332613129932327, -228.6717927865686590 ) ) ;
#12269 = CARTESIAN_POINT ( 'NONE',  ( 6.771176146757415637, 15.60014285904435027, -218.3493856697694753 ) ) ;
#12270 = CARTESIAN_POINT ( 'NONE',  ( -1.243734262319729389, 14.23902626181890518, -226.4313640849764795 ) ) ;
#12271 = VERTEX_POINT ( 'NONE', #9769 ) ;
#12272 = CARTESIAN_POINT ( 'NONE',  ( 18.12061937846576853, -10.14999073105125227, -235.3098052193838612 ) ) ;
#12273 = ORIENTED_EDGE ( 'NONE', *, *, #2906, .T. ) ;
#12274 = CARTESIAN_POINT ( 'NONE',  ( 18.76922974182421555, 13.12635134380198210, -217.8010375391909008 ) ) ;
#12275 = EDGE_CURVE ( 'NONE', #21809, #10093, #22052, .T. ) ;
#12276 = CARTESIAN_POINT ( 'NONE',  ( -20.95553895916151177, 12.88782924195037438, -232.2493899712447956 ) ) ;
#12277 = CARTESIAN_POINT ( 'NONE',  ( -14.30096418567650041, 6.974026439069829664, -228.7941652905285537 ) ) ;
#12278 = CARTESIAN_POINT ( 'NONE',  ( -10.73077095140340376, -23.14408218571897891, -231.4559151628563995 ) ) ;
#12279 = CARTESIAN_POINT ( 'NONE',  ( -10.51143808951550085, 11.41308718311005066, -231.3573069600382439 ) ) ;
#12280 = CARTESIAN_POINT ( 'NONE',  ( -13.12488928717151637, 0.000000000000000000, -103.0000000000000000 ) ) ;
#12281 = CARTESIAN_POINT ( 'NONE',  ( 0.000000000000000000, 0.000000000000000000, -30.00000000000000000 ) ) ;
#12282 = DIRECTION ( 'NONE',  ( -1.000000000000000000, 0.000000000000000000, 0.000000000000000000 ) ) ;
#12283 = AXIS2_PLACEMENT_3D ( 'NONE', #15885, #17344, #11754 ) ;
#12284 = CARTESIAN_POINT ( 'NONE',  ( -15.07599795178976443, 12.40109266655585429, -218.9921934537110815 ) ) ;
#12285 = CARTESIAN_POINT ( 'NONE',  ( 10.90540179105271967, 5.382827416078996841, -224.1493061458977820 ) ) ;
#12286 = CARTESIAN_POINT ( 'NONE',  ( -14.10849459794400751, -0.2436790717799666162, -223.1085195285415921 ) ) ;
#12287 = CARTESIAN_POINT ( 'NONE',  ( -30.94549479715584539, -0.2777009447058255143, -220.3105931650466118 ) ) ;
#12288 = AXIS2_PLACEMENT_3D ( 'NONE', #3106, #18756, #6722 ) ;
#12289 = CARTESIAN_POINT ( 'NONE',  ( -16.30907414568449454, -3.310091733494833655, -231.8954501777161283 ) ) ;
#12290 = CARTESIAN_POINT ( 'NONE',  ( -10.59650102373989533, 7.849913810122476576, -230.0486530042683171 ) ) ;
#12291 = CARTESIAN_POINT ( 'NONE',  ( -15.48425879135615446, -25.29886615046042309, -220.6886037686364261 ) ) ;
#12292 = CARTESIAN_POINT ( 'NONE',  ( 10.85888002857596923, 15.81835858589122878, -232.3913150909872627 ) ) ;
#12293 = CARTESIAN_POINT ( 'NONE',  ( 4.210909054564462295, -12.48022235161367988, -220.2789660014272215 ) ) ;
#12294 = CARTESIAN_POINT ( 'NONE',  ( 14.87928902430193467, -0.2810696969786992683, -227.9872538617268276 ) ) ;
#12295 = CARTESIAN_POINT ( 'NONE',  ( -24.79507334250576278, 6.844873424762779379, -218.1074956078844878 ) ) ;
#12296 =( LENGTH_UNIT ( ) NAMED_UNIT ( * ) SI_UNIT ( .MILLI., .METRE. ) );
#12297 = CARTESIAN_POINT ( 'NONE',  ( 0.4762409465891800919, 16.20008108839776284, -225.9988706007428050 ) ) ;
#12298 = CARTESIAN_POINT ( 'NONE',  ( 22.16968511661519869, 1.542591969257184337, -234.6098499860488573 ) ) ;
#12299 = CIRCLE ( 'NONE', #1866, 17.50000000000007816 ) ;
#12300 = CARTESIAN_POINT ( 'NONE',  ( 21.60524407607017849, 3.028118258437591415, -217.8361640396714449 ) ) ;
#12301 = CARTESIAN_POINT ( 'NONE',  ( 12.49127101283658803, 6.474961340449192804, -221.2149164507559078 ) ) ;
#12302 = CARTESIAN_POINT ( 'NONE',  ( 7.141633727147962851, -29.98958059360777639, -229.8804610602846594 ) ) ;
#12303 = CARTESIAN_POINT ( 'NONE',  ( 14.82579616070250417, 22.96152595385638762, -233.8920860146931489 ) ) ;
#12304 = DIRECTION ( 'NONE',  ( 1.000000000000000000, 0.000000000000000000, 0.000000000000000000 ) ) ;
#12305 = CARTESIAN_POINT ( 'NONE',  ( 0.6837842112036801590, -24.48318360891119028, -216.1006322475167281 ) ) ;
#12306 = CARTESIAN_POINT ( 'NONE',  ( -8.611121136347097860, 17.46802294375265419, -231.5575697815534113 ) ) ;
#12307 = CARTESIAN_POINT ( 'NONE',  ( 7.450672702945051462, 17.42371045663376705, -217.2894981592719432 ) ) ;
#12308 = AXIS2_PLACEMENT_3D ( 'NONE', #12265, #12383, #17560 ) ;
#12309 = CARTESIAN_POINT ( 'NONE',  ( -24.76115377241536208, -2.015397159694146456, -231.8500816169410825 ) ) ;
#12310 = CARTESIAN_POINT ( 'NONE',  ( -15.50322565568834321, 9.749075856218723857, -229.6019304695566916 ) ) ;
#12311 = ADVANCED_FACE ( 'NONE', ( #7975 ), #4250, .T. ) ;
#12312 = CARTESIAN_POINT ( 'NONE',  ( -9.578110717394128670, 23.64032677849093034, -215.7669555765890550 ) ) ;
#12313 = CARTESIAN_POINT ( 'NONE',  ( 24.32561047128371001, 1.769413244618101011, -218.8629106451077462 ) ) ;
#12314 = ORIENTED_EDGE ( 'NONE', *, *, #13126, .F. ) ;
#12315 = CARTESIAN_POINT ( 'NONE',  ( 6.726326701167932853, -14.50135447204537087, -224.8733857281379755 ) ) ;
#12316 = EDGE_LOOP ( 'NONE', ( #11659, #2874, #11884, #1202 ) ) ;
#12317 = CARTESIAN_POINT ( 'NONE',  ( 12.75766869239441803, -12.84633107758633663, -232.0853690516983079 ) ) ;
#12318 = CARTESIAN_POINT ( 'NONE',  ( -6.208492967940078877, 16.71913201805454463, -230.4912298573936766 ) ) ;
#12319 = ORIENTED_EDGE ( 'NONE', *, *, #14661, .T. ) ;
#12320 = CARTESIAN_POINT ( 'NONE',  ( 11.87982377808925527, 10.85265283465803421, -229.5027252913499183 ) ) ;
#12321 = CARTESIAN_POINT ( 'NONE',  ( 27.92729748684602598, -8.572309054117944527, -222.6487661343338686 ) ) ;
#12322 = CARTESIAN_POINT ( 'NONE',  ( -20.76924187596804217, -21.50248317380421170, -228.3679492147379335 ) ) ;
#12323 = CARTESIAN_POINT ( 'NONE',  ( -1.177898122437396333, -26.14463525305933445, -216.8677949074964033 ) ) ;
#12324 = CARTESIAN_POINT ( 'NONE',  ( -3.389634396460917465, 16.42708991135657115, -221.9057377485790994 ) ) ;
#12325 = PLANE ( 'NONE',  #21660 ) ;
#12326 = CARTESIAN_POINT ( 'NONE',  ( 16.23850682336481199, 8.051046992137072422, -219.2473483181185827 ) ) ;
#12327 = CARTESIAN_POINT ( 'NONE',  ( -9.740348021262962064, 16.12529029871877384, -216.4361617420699702 ) ) ;
#12328 = CARTESIAN_POINT ( 'NONE',  ( -8.791002657293931932, 17.82034842365333205, -218.5247019341474584 ) ) ;
#12329 = CIRCLE ( 'NONE', #15555, 2.000000000000001776 ) ;
#12330 =( BOUNDED_SURFACE ( )  B_SPLINE_SURFACE ( 3, 3, ( 
 ( #7062, #3554, #1657, #5460, #3773, #3443, #7173, #8637, #14038, #18868, #10210, #12120, #5347, #17292, #3327, #8531, #17078, #19195, #15395, #12229, #10323, #10432, #8862, #6834, #22243, #1981, #13702, #1868, #20765, #19081, #5127, #17186, #12008, #8749, #303, #1763, #15611, #75, #6946, #10540, #13817, #20656, #3657, #5239, #15726, #20874, #12342, #13930, #18975, #4004, #21217, #9531, #4227, #17868, #11324, #12684, #10880, #5803, #19855, #13008, #4119, #2756, #17757, #14603, #12576, #4329, #16499, #14489, #2430, #10998, #6028, #12796, #21325, #11212, #14383, #18193, #9313, #16174, #6135, #5919, #2320, #17974, #9206, #4441, #2650, #16069, #639, #7515, #19532, #744, #2538, #7620, #16391, #7950, #9637, #5696, #21544, #19642, #11106, #1076, #9415, #16280, #21111, #19419, #855, #7733, #21438, #969, #18079, #12902, #7843, #19749, #14709, #27, #5081, #10491, #5300, #17357, #12074, #1934, #20490, #16917, #8486, #19970, #6897, #1719, #22084, #10277, #13767, #13881, #19036, #14814, #4557, #7009, #18715, #21659, #3613, #141, #11433, #17033, #20606, #4975, #6250, #3279, #22198, #5192, #11850, #18931, #6674, #13124, #12182, #3506, #18302, #15350, #10164, #20719, #2861, #10054, #1608, #1491, #15455, #11962, #8369, #15239, #13546, #20381, #6786, #13655, #18823, #3395, #17143, #8594, #10385, #17246, #1817, #8695, #15561, #7564, #12739, #5409, #3839, #8924, #17809, #17694, #4173, #16007, #21158, #4061, #17586, #8814, #476, #19472, #14105, #11051, #12517, #9257, #19259, #10606, #13992, #17917, #2152, #19367, #15790, #7350, #5746, #3948, #14432, #16116, #9032, #15677, #15896, #689, #10824, #21265, #2263, #19584, #7125, #5858, #369, #10936, #14216, #5529, #257, #7236, #20828, #20942, #12292, #19144, #12408, #3724, #17475, #9146, #2046, #14326, #10720, #21051, #5641, #583, #7458, #12626, #2374, #8006, #18024, #21827, #6080, #14656, #9801, #9586, #21383, #21599, #7677, #16666, #6307, #5973, #14547, #12850, #19692, #21489, #6190, #11268, #20025, #11595, #14986, #9363, #2916, #16449, #1022, #1247, #14759, #13069, #8121, #6416, #2591, #16222, #797, #4612, #14874, #4278, #21715, #19799, #13286, #9691, #19913, #20128, #4716, #2481, #13182, #11158, #7899, #9474, #18137, #16334, #2812, #4502, #1130, #910, #7790, #16552, #11487, #18354, #12955, #4383, #2703, #11381, #18250, #6761, #9918, #17005, #1696, #22173, #20698, #16782, #5275, #17222, #6986, #20466, #6527, #4949, #8568, #3031, #18469, #10251, #13858, #6646, #1584, #8459, #20578, #1357, #117, #11712, #13631, #12049, #10028, #8671, #15432, #20355 ),
 ( #8230, #3482, #2, #21936, #15100, #13396, #20242, #15211, #15327, #11825, #13742, #4836, #15534, #18583, #18906, #3254, #10138, #10359, #5057, #11934, #1795, #3145, #16891, #1465, #8341, #5167, #6870, #22057, #13516, #18691, #18799, #3369, #17117, #7541, #2350, #14411, #9118, #21243, #17561, #13966, #5503, #17330, #12497, #19234, #10801, #19447, #9235, #3926, #17667, #19344, #5723, #7212, #1907, #19013, #15652, #449, #16095, #8791, #14078, #12266, #21136, #21031, #12156, #2237, #15982, #7435, #20916, #3590, #3814, #559, #17451, #10467, #15871, #12603, #344, #20805, #232, #7102, #12384, #7324, #19119, #10697, #14303, #14194, #17785, #4034, #2130, #5382, #3696, #10581, #666, #10910, #2020, #9007, #5619, #8900, #15766, #2892, #2566, #13155, #6164, #18112, #11028, #9775, #8096, #4256, #4586, #16310, #11462, #12826, #19561, #4358, #11356, #9562, #14963, #4148, #5835, #18331, #16640, #7874, #16200, #14633, #18225, #12713, #17895, #19887, #1221, #886, #11241, #2680, #7981, #2458, #9341, #21357, #999, #21689, #19669, #771, #2785, #7763, #7651, #14522, #9450, #9668, #21465, #6057, #12931, #5949, #21576, #20001, #16424, #19777, #11134, #14736, #13041, #4476, #18002, #16527, #1106, #14846, #6281, #21913, #4810, #18882, #5141, #13715, #13606, #1775, #4694, #20329, #15076, #6738, #13489, #10112, #10336, #22254, #16867, #11569, #5032, #20215, #6502, #11686, #8649, #13373, #15299, #3229, #10224, #18558, #21803, #17200, #22149, #15185, #20443, #8432, #3124, #16978, #11909, #20555, #3457, #6390, #18443, #12023, #10004, #13262, #20106, #6847, #3006, #1443, #18774, #8315, #9889, #22029, #6620, #3341, #4925, #17092, #16755, #11801, #1557, #1333, #8205, #18668, #1670, #8545, #15409, #21006, #5254, #5596, #10557, #19423, #426, #5478, #10885, #5702, #17761, #12477, #2325, #20891, #17306, #8878, #20670, #15850, #321, #14171, #534, #12580, #7301, #19323, #3903, #9094, #17427, #12134, #92, #18990, #3792, #4009, #3569, #1997, #15626, #2212, #2107, #15510, #10778, #17646, #15961, #15742, #6963, #7189, #7411, #20780, #13834, #19211, #14281, #3673, #1882, #10446, #8765, #14055, #10676, #206, #12361, #21115, #17540, #7076, #13945, #8987, #5361, #12245, #19096, #4333, #1080, #12906, #13129, #7520, #7954, #9318, #19860, #14607, #5923, #21664, #749, #14388, #16178, #14819, #6254, #14494, #19974, #5808, #2654, #643, #14714, #4561, #2542, #12800, #21329, #16395, #859, #9421, #21549, #2434, #11437, #19646, #4231, #16502, #16285, #12689, #6032, #21221, #18306, #13014, #19536, #4123, #11004, #17872, #11111, #19753 ),
 ( #7625, #11217, #17979, #9210, #4446, #7737, #21442, #18085, #9535, #974, #7848, #6140, #11328, #16073, #18197, #2760, #9641, #9977, #16838, #17065, #15155, #13461, #1642, #15382, #2979, #9749, #1194, #5005, #8405, #14936, #15272, #20186, #6820, #10085, #21997, #20523, #22229, #5112, #22122, #11994, #8286, #4669, #18528, #8071, #3203, #1414, #1526, #10197, #13686, #16950, #6709, #13580, #18745, #4782, #21776, #16612, #6364, #20301, #2865, #13236, #11657, #9863, #11882, #11776, #20082, #20416, #3312, #8519, #3094, #11542, #6592, #18416, #8180, #16728, #4896, #1305, #13344, #15045, #21886, #6475, #18640, #7160, #3540, #10526, #15822, #14026, #2184, #3872, #12218, #5673, #19070, #10752, #20863, #17618, #291, #509, #17173, #9065, #18963, #7271, #1970, #15599, #15932, #10419, #1750, #17280, #7385, #14253, #1854, #21086, #15485, #12328, #10309, #2078, #18854, #3645, #178, #8732, #3759, #17396, #8848, #8958, #12108, #3429, #7047, #13919, #8624, #58, #5446, #6932, #13803, #20754, #5335, #5567, #19183, #20642, #10644, #398, #14140, #15714, #5227, #17511, #20979, #12445, #19295, #16253, #12982, #720, #14360, #17729, #21631, #5893, #828, #19505, #4203, #9505, #7708, #18170, #19829, #12770, #12551, #19618, #4415, #14577, #11299, #21413, #16476, #10855, #2734, #12659, #943, #17949, #9287, #9614, #4095, #2297, #10971, #1053, #7926, #17841, #14789, #9181, #6003, #3981, #18053, #19398, #11082, #16148, #2406, #19725, #2513, #9391, #2622, #5778, #16044, #7594, #14463, #616, #12875, #7491, #4305, #21193, #21296, #16366, #11187, #7820, #14685, #21519, #6111, #3064, #15018, #1499, #15359, #18723, #13099, #6683, #13317, #20158, #20390, #18503, #16812, #4983, #3288, #6338, #19945, #4534, #8378, #11750, #18279, #18616, #1279, #10172, #13434, #9953, #1617, #17041, #8495, #3177, #6223, #11630, #8040, #21858, #11410, #6562, #4751, #4871, #13555, #2840, #20276, #10061, #16925, #22093, #8153, #9722, #16584, #15247, #18386, #1165, #9836, #1388, #11858, #2949, #14908, #13211, #21748, #20056, #4643, #11516, #6447, #8263, #16698, #15130, #21969, #18939, #7244, #264, #12190, #5089, #3848, #2160, #20614, #20950, #10394, #5538, #6906, #13663, #20728, #5418, #3621, #9040, #20499, #22206, #12416, #10728, #1941, #10286, #8703, #12301, #6795, #11969, #14000, #17593, #17254, #5308, #19045, #2053, #18831, #3405, #15463, #17365, #15798, #13775, #19268, #19154, #1826, #17151, #1728, #3514, #3732, #15569, #149, #7017, #8602, #15686, #14114, #10500, #13891, #36, #8821, #7134, #20836, #5200, #10614, #17485, #12083, #8931 ),
 ( #376, #7877, #4480, #4697, #16643, #11244, #21360, #21693, #14636, #16314, #6060, #18446, #890, #9671, #19891, #4589, #21468, #15906, #11572, #16530, #9565, #7984, #2788, #7766, #11359, #14849, #14966, #20109, #3009, #5952, #8099, #19780, #774, #7654, #1225, #12829, #18116, #9453, #1109, #14739, #18228, #14526, #21806, #2683, #19672, #6284, #12934, #4361, #16427, #4259, #1002, #13158, #20004, #11465, #21579, #11137, #18005, #18334, #6167, #2895, #9778, #13044, #6394, #13265, #2569, #13838, #5258, #21916, #1778, #13495, #12138, #20676, #17204, #15080, #11805, #1675, #22033, #18993, #20333, #16982, #8549, #6624, #15413, #16870, #9894, #96, #17097, #16758, #10117, #4929, #15514, #1337, #6966, #18672, #8653, #10228, #22153, #6506, #8208, #13376, #8319, #20218, #3233, #4814, #1447, #11692, #8435, #22257, #13610, #18562, #3127, #10007, #15189, #1561, #11913, #15305, #6742, #6852, #20447, #5036, #13720, #18779, #3345, #20559, #5146, #12027, #18888, #3462, #10340, #21009, #19428, #17431, #16076, #537, #5481, #9214, #12692, #7193, #9097, #20895, #12364, #19214, #20784, #19327, #17764, #8990, #3796, #5365, #429, #10680, #10782, #7081, #325, #7415, #5812, #8883, #3677, #15747, #646, #7523, #2328, #17650, #3573, #8769, #2111, #15853, #19100, #2215, #17543, #14174, #14392, #4012, #7304, #15631, #15964, #2001, #10561, #14060, #10450, #5599, #3906, #12480, #14284, #21118, #17311, #21224, #5706, #12583, #10888, #1886, #212, #13949, #12249, #18310, #1198, #14940, #9321, #11441, #863, #21781, #8075, #4566, #2437, #21446, #11332, #9425, #6368, #7740, #4336, #18203, #16288, #2764, #4234, #19539, #9752, #4450, #4127, #19756, #14612, #2870, #11008, #16616, #6035, #17875, #19864, #9539, #16181, #752, #7628, #17982, #14498, #12909, #21332, #11114, #5926, #18088, #9645, #977, #12805, #19649, #2544, #11220, #2657, #21553, #16400, #7852, #16507, #14718, #6144, #1084, #13018, #7958, #14823, #21668, #6258, #13133, #19979, #6479, #8409, #6824, #4786, #3433, #10201, #15159, #18858, #63, #16842, #18748, #8291, #22002, #6597, #8183, #6714, #5117, #18644, #13465, #15049, #10089, #20304, #20420, #16731, #9981, #17068, #15488, #18531, #13348, #3099, #10314, #17177, #11999, #5009, #13240, #18419, #20085, #4901, #1647, #1418, #4672, #16954, #13690, #11780, #21890, #2983, #11547, #3207, #1531, #20191, #15277, #8522, #22126, #1753, #20528, #13584, #9866, #11886, #8628, #3318, #1309, #15386, #11661, #22233, #21090, #7051, #17621, #12333, #3647, #19401, #20756, #12111, #13921, #5676, #12554, #12220, #10859, #3544, #401 ),
 ( #16047, #10531, #12447, #1972, #8850, #15717, #1858, #7275, #3984, #19186, #294, #8737, #3762, #7162, #14145, #10422, #17398, #3875, #9184, #19072, #5337, #14029, #17735, #2300, #6937, #20982, #13807, #18967, #5450, #181, #5570, #20865, #17514, #20647, #7388, #10647, #17283, #19298, #2082, #8960, #15824, #5230, #10756, #2187, #9068, #15937, #512, #15603, #14257, #16370, #16257, #14688, #9509, #7599, #18057, #21522, #21634, #4537, #18282, #12663, #14792, #4207, #2843, #11413, #7929, #5784, #2517, #6114, #12774, #9725, #11086, #7712, #12985, #19622, #19832, #14582, #19511, #19729, #4098, #6228, #4420, #10976, #17846, #2410, #9292, #17953, #4309, #9395, #18173, #618, #13102, #7494, #1056, #21417, #6007, #19948, #12879, #11191, #14363, #21196, #724, #16153, #14467, #2737, #11302, #21301, #9617, #833, #5898, #7823, #2628, #947, #16479, #18834, #13557, #11971, #21971, #18389, #9955, #21751, #16927, #1390, #15249, #1619, #13665, #8380, #22096, #1501, #10174, #11634, #6341, #1168, #20059, #4873, #20501, #13214, #18505, #16702, #3290, #3179, #3408, #6685, #20392, #11860, #3067, #16587, #8265, #4985, #21861, #8045, #20278, #17044, #4754, #2953, #4646, #14911, #16814, #11752, #1282, #15132, #18725, #18618, #22208, #8497, #6564, #11519, #13438, #15361, #10063, #6797, #5091, #9841, #8156, #15021, #6450, #13320, #20160, #7021, #486, #1828, #15465, #10396, #9042, #2162, #15571, #14229, #6908, #3734, #1730, #15800, #5652, #3623, #13893, #151, #17487, #1943, #10502, #378, #3516, #7360, #20730, #5310, #17595, #12192, #7246, #12529, #19048, #17256, #17367, #21064, #15908, #19377, #2055, #10288, #38, #8823, #8705, #8933, #15688, #20838, #17153, #10730, #266, #13777, #14117, #7136, #14002, #5421, #8604, #12303, #10618, #19156, #20952, #5540, #20617, #5202, #12420, #19271, #3850, #12085, #18941, #21393, #2603, #2714, #7908, #21610, #16019, #18147, #7575, #6202, #14771, #11278, #9156, #5867, #18034, #16126, #13079, #14441, #11060, #9484, #699, #16345, #10947, #3958, #16459, #11167, #10833, #4184, #21276, #9596, #17706, #1034, #12748, #2272, #4288, #16232, #594, #7467, #14336, #2384, #21169, #19597, #5756, #17821, #12636, #2492, #921, #7687, #19484, #4071, #9268, #17929, #9372, #5985, #808, #14556, #7801, #12859, #19703, #14666, #21500, #6090, #12965, #19809, #4394, #18259, #1595, #13191, #15111, #13531, #11497, #10151, #16903, #21837, #3267, #6774, #1256, #3158, #14998, #6427, #13297, #14883, #13411, #11839, #3042, #20138, #21724, #16792, #4729, #4849, #1142, #2926, #22186, #1367, #20369, #8132 ),
 ( #18704, #11608, #17020, #4623, #11391, #18480, #10042, #8243, #19923, #2823, #4511, #8472, #15339, #21948, #8019, #9930, #1479, #9703, #16563, #11727, #6317, #6540, #20253, #18595, #22070, #20035, #18366, #9814, #8355, #4960, #16676, #15226, #6660, #15548, #19245, #460, #17234, #19129, #8682, #127, #6995, #8580, #7111, #5515, #19022, #13867, #15444, #10476, #20708, #20815, #17130, #10370, #10592, #15882, #18918, #13753, #3494, #10707, #3825, #12394, #5392, #13643, #18810, #12166, #6884, #12277, #5286, #1919, #2140, #14088, #3600, #3381, #3709, #12060, #20592, #1805, #20479, #5178, #13975, #17341, #2031, #8800, #5070, #9017, #17461, #15661, #8910, #242, #15776, #355, #7223, #17571, #11946, #10262, #1706, #14, #20928, #2690, #18123, #14644, #12507, #9244, #21367, #19457, #16434, #10922, #14419, #5959, #4045, #12836, #14313, #7337, #19786, #14533, #21040, #5844, #19680, #11038, #9572, #5630, #14204, #6069, #19354, #9350, #17678, #16104, #4266, #3936, #10811, #11144, #2250, #17794, #12723, #19570, #9461, #9130, #11253, #569, #2468, #897, #21145, #4369, #18012, #676, #12941, #15993, #2360, #2578, #7551, #21252, #4157, #7445, #782, #21475, #17904, #16210, #5733, #7663, #16321, #7774, #12612, #1117, #6403, #15088, #9679, #18236, #16538, #1345, #9903, #3018, #8107, #21924, #14746, #20011, #11367, #1233, #13166, #18341, #8216, #18455, #7993, #21587, #21814, #2796, #14858, #21701, #1009, #6292, #14973, #2902, #20115, #4597, #7884, #6176, #13273, #11473, #4704, #11581, #9787, #16766, #13055, #19900, #4488, #16652, #9440, #990, #2341, #658, #7754, #1096, #16088, #14514, #19553, #6155, #6047, #14837, #4348, #9553, #14729, #5940, #19440, #11126, #7864, #2450, #21680, #878, #19879, #7641, #21235, #9227, #6271, #12818, #14626, #4141, #17994, #16415, #21458, #2776, #4465, #19661, #4026, #16518, #11232, #18103, #19768, #2557, #16302, #21566, #7535, #14404, #12922, #7969, #5827, #21346, #11020, #13031, #2670, #10903, #11345, #18216, #9659, #4246, #17777, #12706, #17887, #9333, #16193, #765, #13597, #1325, #14955, #18323, #22246, #6492, #1433, #20097, #4801, #10103, #8306, #18762, #20434, #13362, #13146, #20206, #5023, #15173, #11899, #16857, #17082, #11454, #3331, #13252, #1545, #18548, #9881, #10214, #4686, #2883, #11559, #1660, #8535, #18434, #15399, #9764, #6611, #4578, #18660, #19991, #11677, #16745, #2997, #20319, #3115, #9995, #3220, #6380, #16630, #8196, #15064, #1213, #22018, #8088, #13480, #21794, #21904, #16967, #4917, #11793, #8423, #15290, #22139, #6729, #15615, #2095, #15949, #19312 ),
 ( #20769, #17416, #17634, #7289, #1871, #12014, #12349, #5242, #6951, #18979, #9082, #13823, #308, #10546, #17528, #12123, #6838, #2201, #7179, #195, #20880, #15731, #20660, #1986, #5586, #13706, #8866, #17189, #7065, #19201, #20543, #5130, #5466, #18872, #17296, #12234, #19085, #8975, #3446, #10768, #80, #14044, #415, #3558, #3890, #3781, #8754, #12466, #10327, #10436, #10663, #13934, #5351, #3661, #1766, #15839, #20996, #14160, #8640, #15501, #19635, #737, #7725, #3997, #19525, #19742, #2749, #5796, #633, #12677, #19847, #6127, #14702, #14596, #9630, #5689, #21315, #16063, #21431, #14481, #11099, #11316, #962, #17860, #12568, #6021, #21210, #7509, #4112, #524, #14376, #16272, #4219, #11205, #10991, #7402, #18186, #847, #16167, #12894, #9408, #2423, #17967, #4322, #21536, #4434, #19413, #9306, #7613, #5912, #14272, #21104, #7836, #10873, #12789, #18071, #2531, #17749, #2643, #9523, #16383, #13001, #2313, #9198, #16492, #6697, #1403, #11870, #16717, #11531, #22110, #4994, #13569, #13225, #1515, #16825, #6464, #21650, #20405, #18734, #14924, #15261, #4658, #3300, #1181, #7943, #15034, #21986, #20175, #1069, #14807, #6243, #20290, #13117, #19963, #4769, #4550, #11426, #18404, #16600, #3191, #3083, #18295, #8275, #6579, #11765, #2966, #2854, #8168, #4885, #21764, #9738, #11645, #16939, #9852, #8059, #6353, #20071, #1294, #18516, #21875, #13333, #13449, #9966, #15144, #8393, #18629, #10074, #3526, #2370, #5321, #9252, #13905, #14428, #8508, #16112, #10298, #21154, #15584, #6920, #685, #1739, #15371, #17162, #7559, #21261, #15474, #5852, #6809, #3944, #1630, #16003, #12735, #10405, #13789, #47, #17689, #1839, #17267, #578, #3418, #19579, #20627, #5213, #17803, #8717, #13675, #7032, #22218, #10184, #14321, #20512, #5102, #11982, #18843, #12095, #20740, #18950, #5742, #17053, #8613, #162, #10932, #12202, #19363, #10820, #2258, #9141, #7453, #12621, #19466, #4055, #2477, #6301, #9686, #16218, #16546, #21483, #8116, #11376, #16443, #21821, #16659, #6411, #1124, #13281, #9580, #5969, #19794, #9358, #4497, #11261, #19688, #21594, #2806, #2910, #14981, #792, #18019, #4167, #11046, #2586, #9795, #14651, #1242, #11153, #17912, #2698, #8001, #7892, #7671, #14542, #21378, #12845, #4274, #6185, #9468, #12950, #14866, #16329, #905, #18244, #7785, #6076, #1016, #14753, #13174, #4377, #18131, #13062, #19908, #20019, #21709, #4606, #11481, #18348, #3476, #6980, #1460, #3363, #15206, #22051, #6641, #15095, #13626, #12043, #3248, #13511, #21932, #17000, #20349, #5052, #1352, #16885, #17112, #112 ) ),
 .UNSPECIFIED., .T., .F., .F. ) 
 B_SPLINE_SURFACE_WITH_KNOTS ( ( 4, 3, 4 ),
 ( 4, 2, 2, 2, 2, 2, 2, 2, 2, 2, 2, 2, 2, 2, 2, 2, 2, 2, 2, 2, 2, 2, 2, 2, 2, 2, 2, 2, 2, 2, 2, 2, 2, 2, 2, 2, 2, 2, 2, 2, 2, 2, 2, 2, 2, 2, 2, 2, 2, 2, 2, 2, 2, 2, 2, 2, 2, 2, 2, 2, 2, 2, 2, 2, 2, 2, 2, 2, 2, 2, 2, 2, 2, 2, 2, 2, 2, 2, 2, 2, 2, 2, 2, 2, 2, 2, 2, 2, 2, 2, 2, 2, 2, 2, 2, 2, 2, 2, 2, 2, 2, 2, 2, 2, 2, 2, 2, 2, 2, 2, 2, 2, 2, 2, 2, 2, 2, 2, 2, 2, 2, 2, 2, 2, 2, 2, 2, 2, 2, 2, 2, 2, 2, 2, 2, 2, 2, 2, 2, 2, 2, 2, 2, 2, 2, 2, 2, 2, 2, 2, 2, 2, 2, 2, 2, 2, 2, 2, 2, 2, 2, 2, 2, 2, 2, 2, 2, 4 ),
 ( 0.000000000000000000, 0.5000000000000000000, 1.000000000000000000 ),
 ( 0.000000000000000000, 0.001952908952989333875, 0.003905817905978667751, 0.007323408573709997045, 0.01074099924144132634, 0.01415858990917265650, 0.01586738524303832332, 0.01757618057690398666, 0.02099377124463531682, 0.02441136191236664699, 0.02782895258009797368, 0.03124654324782930384, 0.03466413391556063400, 0.03808172458329196070, 0.04149931525102329433, 0.04491690591875462102, 0.04662570125262028436, 0.04833449658648594771, 0.05175208725421727440, 0.05346088258808293775, 0.05516967792194860110, 0.05858726858967993473, 0.06200485925741126836, 0.06542244992514259505, 0.06884004059287393562, 0.07225763126060526231, 0.07567522192833658901, 0.07909281259606792958, 0.08251040326379925627, 0.08421919859766491268, 0.08592799393153058296, 0.08934558459926195129, 0.09276317526699331961, 0.09447197060085900377, 0.09618076593472468794, 0.09959835660245604239, 0.1030159472701873968, 0.1064335379379187652, 0.1098511286056501335, 0.1132687192733815018, 0.1166863099411127869, 0.1201039006088440858, 0.1235214912765753847, 0.1252302866104410273, 0.1269390819443066698, 0.1303566726120379826, 0.1320654679459036251, 0.1337742632797692677, 0.1371918539475005527, 0.1406094446152318378, 0.1440270352829631784, 0.1474446259506944912, 0.1508622166184258040, 0.1542798072861571446, 0.1576973979538884851, 0.1611149886216198257, 0.1645325792893511663, 0.1679501699570824791, 0.1713677606248137919, 0.1747853512925451325, 0.1764941466264108028, 0.1782029419602764730, 0.1816205326280078136, 0.1850381232957391542, 0.1884557139634704670, 0.1918733046312017798, 0.1952908952989331204, 0.1987084859666644610, 0.2021260766343957738, 0.2055436673021270866, 0.2072524626359927569, 0.2089612579698584272, 0.2123788486375897677, 0.2140876439714554380, 0.2157964393053211083, 0.2192140299730524489, 0.2226316206407837617, 0.2260492113085151300, 0.2294668019762464706, 0.2328843926439778111, 0.2363019833117091517, 0.2397195739794404923, 0.2431371646471718329, 0.2465547553149031734, 0.2499723459826345140, 0.2533899366503657991, 0.2568075273180971396, 0.2602251179858284802, 0.2636427086535597653, 0.2670602993212910503, 0.2704778899890223909, 0.2738954806567537315, 0.2773130713244850165, 0.2807306619922163571, 0.2841482526599476977, 0.2858570479938133957, 0.2875658433276790382, 0.2909834339954103788, 0.2926922293292760768, 0.2944010246631417194, 0.2978186153308730599, 0.3012362059986043450, 0.3046537966663356856, 0.3080713873340670261, 0.3114889780017983112, 0.3149065686695296518, 0.3183241593372609923, 0.3217417500049923329, 0.3234505453388579754, 0.3251593406727236735, 0.3285769313404549585, 0.3319945220081862991, 0.3354121126759176397, 0.3388297033436489247, 0.3422472940113802653, 0.3456648846791116059, 0.3490824753468429464, 0.3525000660145742870, 0.3559176566823056276, 0.3593352473500369682, 0.3627528380177683087, 0.3661704286854996493, 0.3695880193532309343, 0.3730056100209622749, 0.3747144053548279174, 0.3764232006886936155, 0.3798407913564249005, 0.3832583820241562411, 0.3866759726918875817, 0.3900935633596189223, 0.3935111540273502628, 0.3969287446950816034, 0.4003463353628129440, 0.4037639260305442845, 0.4054727213644099271, 0.4071815166982756251, 0.4105991073660069102, 0.4140166980337382507, 0.4157254933676038933, 0.4174342887014695913, 0.4208518793692008764, 0.4242694700369322169, 0.4276870607046635575, 0.4311046513723948981, 0.4345222420401262386, 0.4379398327078575237, 0.4413574233755888643, 0.4447750140433202048, 0.4464838093771859029, 0.4481926047110515454, 0.4516101953787828860, 0.4533189907126485840, 0.4550277860465142266, 0.4584453767142455671, 0.4618629673819769077, 0.4652805580497082483, 0.4686981487174395888, 0.4721157393851709294, 0.4755333300529022145, 0.4789509207206335550, 0.4823685113883648956, 0.4840773067222305381, 0.4857861020560961807, 0.4892036927238275212, 0.4926212833915588618, 0.4960388740592901469, 0.4979917830122794764, 0.4999446919652688059 ),
 .UNSPECIFIED. ) 
 GEOMETRIC_REPRESENTATION_ITEM ( )  RATIONAL_B_SPLINE_SURFACE ( (
 ( 1.000000000000000000, 1.000000000000000000, 1.000000000000000000, 1.000000000000000000, 1.000000000000000000, 1.000000000000000000, 1.000000000000000000, 1.000000000000000000, 1.000000000000000000, 1.000000000000000000, 1.000000000000000000, 1.000000000000000000, 1.000000000000000000, 1.000000000000000000, 1.000000000000000000, 1.000000000000000000, 1.000000000000000000, 1.000000000000000000, 1.000000000000000000, 1.000000000000000000, 1.000000000000000000, 1.000000000000000000, 1.000000000000000000, 1.000000000000000000, 1.000000000000000000, 1.000000000000000000, 1.000000000000000000, 1.000000000000000000, 1.000000000000000000, 1.000000000000000000, 1.000000000000000000, 1.000000000000000000, 1.000000000000000000, 1.000000000000000000, 1.000000000000000000, 1.000000000000000000, 1.000000000000000000, 1.000000000000000000, 1.000000000000000000, 1.000000000000000000, 1.000000000000000000, 1.000000000000000000, 1.000000000000000000, 1.000000000000000000, 1.000000000000000000, 1.000000000000000000, 1.000000000000000000, 1.000000000000000000, 1.000000000000000000, 1.000000000000000000, 1.000000000000000000, 1.000000000000000000, 1.000000000000000000, 1.000000000000000000, 1.000000000000000000, 1.000000000000000000, 1.000000000000000000, 1.000000000000000000, 1.000000000000000000, 1.000000000000000000, 1.000000000000000000, 1.000000000000000000, 1.000000000000000000, 1.000000000000000000, 1.000000000000000000, 1.000000000000000000, 1.000000000000000000, 1.000000000000000000, 1.000000000000000000, 1.000000000000000000, 1.000000000000000000, 1.000000000000000000, 1.000000000000000000, 1.000000000000000000, 1.000000000000000000, 1.000000000000000000, 1.000000000000000000, 1.000000000000000000, 1.000000000000000000, 1.000000000000000000, 1.000000000000000000, 1.000000000000000000, 1.000000000000000000, 1.000000000000000000, 1.000000000000000000, 1.000000000000000000, 1.000000000000000000, 1.000000000000000000, 1.000000000000000000, 1.000000000000000000, 1.000000000000000000, 1.000000000000000000, 1.000000000000000000, 1.000000000000000000, 1.000000000000000000, 1.000000000000000000, 1.000000000000000000, 1.000000000000000000, 1.000000000000000000, 1.000000000000000000, 1.000000000000000000, 1.000000000000000000, 1.000000000000000000, 1.000000000000000000, 1.000000000000000000, 1.000000000000000000, 1.000000000000000000, 1.000000000000000000, 1.000000000000000000, 1.000000000000000000, 1.000000000000000000, 1.000000000000000000, 1.000000000000000000, 1.000000000000000000, 1.000000000000000000, 1.000000000000000000, 1.000000000000000000, 1.000000000000000000, 1.000000000000000000, 1.000000000000000000, 1.000000000000000000, 1.000000000000000000, 1.000000000000000000, 1.000000000000000000, 1.000000000000000000, 1.000000000000000000, 1.000000000000000000, 1.000000000000000000, 1.000000000000000000, 1.000000000000000000, 1.000000000000000000, 1.000000000000000000, 1.000000000000000000, 1.000000000000000000, 1.000000000000000000, 1.000000000000000000, 1.000000000000000000, 1.000000000000000000, 1.000000000000000000, 1.000000000000000000, 1.000000000000000000, 1.000000000000000000, 1.000000000000000000, 1.000000000000000000, 1.000000000000000000, 1.000000000000000000, 1.000000000000000000, 1.000000000000000000, 1.000000000000000000, 1.000000000000000000, 1.000000000000000000, 1.000000000000000000, 1.000000000000000000, 1.000000000000000000, 1.000000000000000000, 1.000000000000000000, 1.000000000000000000, 1.000000000000000000, 1.000000000000000000, 1.000000000000000000, 1.000000000000000000, 1.000000000000000000, 1.000000000000000000, 1.000000000000000000, 1.000000000000000000, 1.000000000000000000, 1.000000000000000000, 1.000000000000000000, 1.000000000000000000, 1.000000000000000000, 1.000000000000000000, 1.000000000000000000, 1.000000000000000000, 1.000000000000000000, 1.000000000000000000, 1.000000000000000000, 1.000000000000000000, 1.000000000000000000, 1.000000000000000000, 1.000000000000000000, 1.000000000000000000, 1.000000000000000000, 1.000000000000000000, 1.000000000000000000, 1.000000000000000000, 1.000000000000000000, 1.000000000000000000, 1.000000000000000000, 1.000000000000000000, 1.000000000000000000, 1.000000000000000000, 1.000000000000000000, 1.000000000000000000, 1.000000000000000000, 1.000000000000000000, 1.000000000000000000, 1.000000000000000000, 1.000000000000000000, 1.000000000000000000, 1.000000000000000000, 1.000000000000000000, 1.000000000000000000, 1.000000000000000000, 1.000000000000000000, 1.000000000000000000, 1.000000000000000000, 1.000000000000000000, 1.000000000000000000, 1.000000000000000000, 1.000000000000000000, 1.000000000000000000, 1.000000000000000000, 1.000000000000000000, 1.000000000000000000, 1.000000000000000000, 1.000000000000000000, 1.000000000000000000, 1.000000000000000000, 1.000000000000000000, 1.000000000000000000, 1.000000000000000000, 1.000000000000000000, 1.000000000000000000, 1.000000000000000000, 1.000000000000000000, 1.000000000000000000, 1.000000000000000000, 1.000000000000000000, 1.000000000000000000, 1.000000000000000000, 1.000000000000000000, 1.000000000000000000, 1.000000000000000000, 1.000000000000000000, 1.000000000000000000, 1.000000000000000000, 1.000000000000000000, 1.000000000000000000, 1.000000000000000000, 1.000000000000000000, 1.000000000000000000, 1.000000000000000000, 1.000000000000000000, 1.000000000000000000, 1.000000000000000000, 1.000000000000000000, 1.000000000000000000, 1.000000000000000000, 1.000000000000000000, 1.000000000000000000, 1.000000000000000000, 1.000000000000000000, 1.000000000000000000, 1.000000000000000000, 1.000000000000000000, 1.000000000000000000, 1.000000000000000000, 1.000000000000000000, 1.000000000000000000, 1.000000000000000000, 1.000000000000000000, 1.000000000000000000, 1.000000000000000000, 1.000000000000000000, 1.000000000000000000, 1.000000000000000000, 1.000000000000000000, 1.000000000000000000, 1.000000000000000000, 1.000000000000000000, 1.000000000000000000, 1.000000000000000000, 1.000000000000000000, 1.000000000000000000, 1.000000000000000000, 1.000000000000000000, 1.000000000000000000, 1.000000000000000000, 1.000000000000000000, 1.000000000000000000, 1.000000000000000000, 1.000000000000000000, 1.000000000000000000, 1.000000000000000000, 1.000000000000000000, 1.000000000000000000, 1.000000000000000000, 1.000000000000000000, 1.000000000000000000, 1.000000000000000000, 1.000000000000000000, 1.000000000000000000, 1.000000000000000000, 1.000000000000000000, 1.000000000000000000, 1.000000000000000000, 1.000000000000000000, 1.000000000000000000, 1.000000000000000000, 1.000000000000000000, 1.000000000000000000, 1.000000000000000000, 1.000000000000000000, 1.000000000000000000, 1.000000000000000000, 1.000000000000000000, 1.000000000000000000, 1.000000000000000000, 1.000000000000000000, 1.000000000000000000, 1.000000000000000000, 1.000000000000000000, 1.000000000000000000, 1.000000000000000000, 1.000000000000000000, 1.000000000000000000, 1.000000000000000000, 1.000000000000000000, 1.000000000000000000, 1.000000000000000000, 1.000000000000000000, 1.000000000000000000, 1.000000000000000000, 1.000000000000000000, 1.000000000000000000, 1.000000000000000000, 1.000000000000000000, 1.000000000000000000, 1.000000000000000000, 1.000000000000000000, 1.000000000000000000, 1.000000000000000000, 1.000000000000000000, 1.000000000000000000, 1.000000000000000000, 1.000000000000000000),
 ( 0.3333333333333333703, 0.3333333333333333703, 0.3333333333333333703, 0.3333333333333333703, 0.3333333333333333703, 0.3333333333333333703, 0.3333333333333333703, 0.3333333333333333703, 0.3333333333333333703, 0.3333333333333333703, 0.3333333333333333703, 0.3333333333333333703, 0.3333333333333333703, 0.3333333333333333703, 0.3333333333333333703, 0.3333333333333333703, 0.3333333333333333703, 0.3333333333333333703, 0.3333333333333333703, 0.3333333333333333703, 0.3333333333333333703, 0.3333333333333333703, 0.3333333333333333703, 0.3333333333333333703, 0.3333333333333333703, 0.3333333333333333703, 0.3333333333333333703, 0.3333333333333333703, 0.3333333333333333703, 0.3333333333333333703, 0.3333333333333333703, 0.3333333333333333703, 0.3333333333333333703, 0.3333333333333333703, 0.3333333333333333703, 0.3333333333333333703, 0.3333333333333333703, 0.3333333333333333703, 0.3333333333333333703, 0.3333333333333333703, 0.3333333333333333703, 0.3333333333333333703, 0.3333333333333333703, 0.3333333333333333703, 0.3333333333333333703, 0.3333333333333333703, 0.3333333333333333703, 0.3333333333333333703, 0.3333333333333333703, 0.3333333333333333703, 0.3333333333333333703, 0.3333333333333333703, 0.3333333333333333703, 0.3333333333333333703, 0.3333333333333333703, 0.3333333333333333703, 0.3333333333333333703, 0.3333333333333333703, 0.3333333333333333703, 0.3333333333333333703, 0.3333333333333333703, 0.3333333333333333703, 0.3333333333333333703, 0.3333333333333333703, 0.3333333333333333703, 0.3333333333333333703, 0.3333333333333333703, 0.3333333333333333703, 0.3333333333333333703, 0.3333333333333333703, 0.3333333333333333703, 0.3333333333333333703, 0.3333333333333333703, 0.3333333333333333703, 0.3333333333333333703, 0.3333333333333333703, 0.3333333333333333703, 0.3333333333333333703, 0.3333333333333333703, 0.3333333333333333703, 0.3333333333333333703, 0.3333333333333333703, 0.3333333333333333703, 0.3333333333333333703, 0.3333333333333333703, 0.3333333333333333703, 0.3333333333333333703, 0.3333333333333333703, 0.3333333333333333703, 0.3333333333333333703, 0.3333333333333333703, 0.3333333333333333703, 0.3333333333333333703, 0.3333333333333333703, 0.3333333333333333703, 0.3333333333333333703, 0.3333333333333333703, 0.3333333333333333703, 0.3333333333333333703, 0.3333333333333333703, 0.3333333333333333703, 0.3333333333333333703, 0.3333333333333333703, 0.3333333333333333703, 0.3333333333333333703, 0.3333333333333333703, 0.3333333333333333703, 0.3333333333333333703, 0.3333333333333333703, 0.3333333333333333703, 0.3333333333333333703, 0.3333333333333333703, 0.3333333333333333703, 0.3333333333333333703, 0.3333333333333333703, 0.3333333333333333703, 0.3333333333333333703, 0.3333333333333333703, 0.3333333333333333703, 0.3333333333333333703, 0.3333333333333333703, 0.3333333333333333703, 0.3333333333333333703, 0.3333333333333333703, 0.3333333333333333703, 0.3333333333333333703, 0.3333333333333333703, 0.3333333333333333703, 0.3333333333333333703, 0.3333333333333333703, 0.3333333333333333703, 0.3333333333333333703, 0.3333333333333333703, 0.3333333333333333703, 0.3333333333333333703, 0.3333333333333333703, 0.3333333333333333703, 0.3333333333333333703, 0.3333333333333333703, 0.3333333333333333703, 0.3333333333333333703, 0.3333333333333333703, 0.3333333333333333703, 0.3333333333333333703, 0.3333333333333333703, 0.3333333333333333703, 0.3333333333333333703, 0.3333333333333333703, 0.3333333333333333703, 0.3333333333333333703, 0.3333333333333333703, 0.3333333333333333703, 0.3333333333333333703, 0.3333333333333333703, 0.3333333333333333703, 0.3333333333333333703, 0.3333333333333333703, 0.3333333333333333703, 0.3333333333333333703, 0.3333333333333333703, 0.3333333333333333703, 0.3333333333333333703, 0.3333333333333333703, 0.3333333333333333703, 0.3333333333333333703, 0.3333333333333333703, 0.3333333333333333703, 0.3333333333333333703, 0.3333333333333333703, 0.3333333333333333703, 0.3333333333333333703, 0.3333333333333333703, 0.3333333333333333703, 0.3333333333333333703, 0.3333333333333333703, 0.3333333333333333703, 0.3333333333333333703, 0.3333333333333333703, 0.3333333333333333703, 0.3333333333333333703, 0.3333333333333333703, 0.3333333333333333703, 0.3333333333333333703, 0.3333333333333333703, 0.3333333333333333703, 0.3333333333333333703, 0.3333333333333333703, 0.3333333333333333703, 0.3333333333333333703, 0.3333333333333333703, 0.3333333333333333703, 0.3333333333333333703, 0.3333333333333333703, 0.3333333333333333703, 0.3333333333333333703, 0.3333333333333333703, 0.3333333333333333703, 0.3333333333333333703, 0.3333333333333333703, 0.3333333333333333703, 0.3333333333333333703, 0.3333333333333333703, 0.3333333333333333703, 0.3333333333333333703, 0.3333333333333333703, 0.3333333333333333703, 0.3333333333333333703, 0.3333333333333333703, 0.3333333333333333703, 0.3333333333333333703, 0.3333333333333333703, 0.3333333333333333703, 0.3333333333333333703, 0.3333333333333333703, 0.3333333333333333703, 0.3333333333333333703, 0.3333333333333333703, 0.3333333333333333703, 0.3333333333333333703, 0.3333333333333333703, 0.3333333333333333703, 0.3333333333333333703, 0.3333333333333333703, 0.3333333333333333703, 0.3333333333333333703, 0.3333333333333333703, 0.3333333333333333703, 0.3333333333333333703, 0.3333333333333333703, 0.3333333333333333703, 0.3333333333333333703, 0.3333333333333333703, 0.3333333333333333703, 0.3333333333333333703, 0.3333333333333333703, 0.3333333333333333703, 0.3333333333333333703, 0.3333333333333333703, 0.3333333333333333703, 0.3333333333333333703, 0.3333333333333333703, 0.3333333333333333703, 0.3333333333333333703, 0.3333333333333333703, 0.3333333333333333703, 0.3333333333333333703, 0.3333333333333333703, 0.3333333333333333703, 0.3333333333333333703, 0.3333333333333333703, 0.3333333333333333703, 0.3333333333333333703, 0.3333333333333333703, 0.3333333333333333703, 0.3333333333333333703, 0.3333333333333333703, 0.3333333333333333703, 0.3333333333333333703, 0.3333333333333333703, 0.3333333333333333703, 0.3333333333333333703, 0.3333333333333333703, 0.3333333333333333703, 0.3333333333333333703, 0.3333333333333333703, 0.3333333333333333703, 0.3333333333333333703, 0.3333333333333333703, 0.3333333333333333703, 0.3333333333333333703, 0.3333333333333333703, 0.3333333333333333703, 0.3333333333333333703, 0.3333333333333333703, 0.3333333333333333703, 0.3333333333333333703, 0.3333333333333333703, 0.3333333333333333703, 0.3333333333333333703, 0.3333333333333333703, 0.3333333333333333703, 0.3333333333333333703, 0.3333333333333333703, 0.3333333333333333703, 0.3333333333333333703, 0.3333333333333333703, 0.3333333333333333703, 0.3333333333333333703, 0.3333333333333333703, 0.3333333333333333703, 0.3333333333333333703, 0.3333333333333333703, 0.3333333333333333703, 0.3333333333333333703, 0.3333333333333333703, 0.3333333333333333703, 0.3333333333333333703, 0.3333333333333333703, 0.3333333333333333703, 0.3333333333333333703, 0.3333333333333333703, 0.3333333333333333703, 0.3333333333333333703, 0.3333333333333333703, 0.3333333333333333703, 0.3333333333333333703, 0.3333333333333333703, 0.3333333333333333703, 0.3333333333333333703, 0.3333333333333333703, 0.3333333333333333703, 0.3333333333333333703, 0.3333333333333333703, 0.3333333333333333703, 0.3333333333333333703, 0.3333333333333333703, 0.3333333333333333703, 0.3333333333333333703, 0.3333333333333333703, 0.3333333333333333703, 0.3333333333333333703, 0.3333333333333333703, 0.3333333333333333703, 0.3333333333333333703, 0.3333333333333333703, 0.3333333333333333703, 0.3333333333333333703, 0.3333333333333333703, 0.3333333333333333703, 0.3333333333333333703, 0.3333333333333333703, 0.3333333333333333703, 0.3333333333333333703, 0.3333333333333333703, 0.3333333333333333703, 0.3333333333333333703),
 ( 0.3333333333333333703, 0.3333333333333333703, 0.3333333333333333703, 0.3333333333333333703, 0.3333333333333333703, 0.3333333333333333703, 0.3333333333333333703, 0.3333333333333333703, 0.3333333333333333703, 0.3333333333333333703, 0.3333333333333333703, 0.3333333333333333703, 0.3333333333333333703, 0.3333333333333333703, 0.3333333333333333703, 0.3333333333333333703, 0.3333333333333333703, 0.3333333333333333703, 0.3333333333333333703, 0.3333333333333333703, 0.3333333333333333703, 0.3333333333333333703, 0.3333333333333333703, 0.3333333333333333703, 0.3333333333333333703, 0.3333333333333333703, 0.3333333333333333703, 0.3333333333333333703, 0.3333333333333333703, 0.3333333333333333703, 0.3333333333333333703, 0.3333333333333333703, 0.3333333333333333703, 0.3333333333333333703, 0.3333333333333333703, 0.3333333333333333703, 0.3333333333333333703, 0.3333333333333333703, 0.3333333333333333703, 0.3333333333333333703, 0.3333333333333333703, 0.3333333333333333703, 0.3333333333333333703, 0.3333333333333333703, 0.3333333333333333703, 0.3333333333333333703, 0.3333333333333333703, 0.3333333333333333703, 0.3333333333333333703, 0.3333333333333333703, 0.3333333333333333703, 0.3333333333333333703, 0.3333333333333333703, 0.3333333333333333703, 0.3333333333333333703, 0.3333333333333333703, 0.3333333333333333703, 0.3333333333333333703, 0.3333333333333333703, 0.3333333333333333703, 0.3333333333333333703, 0.3333333333333333703, 0.3333333333333333703, 0.3333333333333333703, 0.3333333333333333703, 0.3333333333333333703, 0.3333333333333333703, 0.3333333333333333703, 0.3333333333333333703, 0.3333333333333333703, 0.3333333333333333703, 0.3333333333333333703, 0.3333333333333333703, 0.3333333333333333703, 0.3333333333333333703, 0.3333333333333333703, 0.3333333333333333703, 0.3333333333333333703, 0.3333333333333333703, 0.3333333333333333703, 0.3333333333333333703, 0.3333333333333333703, 0.3333333333333333703, 0.3333333333333333703, 0.3333333333333333703, 0.3333333333333333703, 0.3333333333333333703, 0.3333333333333333703, 0.3333333333333333703, 0.3333333333333333703, 0.3333333333333333703, 0.3333333333333333703, 0.3333333333333333703, 0.3333333333333333703, 0.3333333333333333703, 0.3333333333333333703, 0.3333333333333333703, 0.3333333333333333703, 0.3333333333333333703, 0.3333333333333333703, 0.3333333333333333703, 0.3333333333333333703, 0.3333333333333333703, 0.3333333333333333703, 0.3333333333333333703, 0.3333333333333333703, 0.3333333333333333703, 0.3333333333333333703, 0.3333333333333333703, 0.3333333333333333703, 0.3333333333333333703, 0.3333333333333333703, 0.3333333333333333703, 0.3333333333333333703, 0.3333333333333333703, 0.3333333333333333703, 0.3333333333333333703, 0.3333333333333333703, 0.3333333333333333703, 0.3333333333333333703, 0.3333333333333333703, 0.3333333333333333703, 0.3333333333333333703, 0.3333333333333333703, 0.3333333333333333703, 0.3333333333333333703, 0.3333333333333333703, 0.3333333333333333703, 0.3333333333333333703, 0.3333333333333333703, 0.3333333333333333703, 0.3333333333333333703, 0.3333333333333333703, 0.3333333333333333703, 0.3333333333333333703, 0.3333333333333333703, 0.3333333333333333703, 0.3333333333333333703, 0.3333333333333333703, 0.3333333333333333703, 0.3333333333333333703, 0.3333333333333333703, 0.3333333333333333703, 0.3333333333333333703, 0.3333333333333333703, 0.3333333333333333703, 0.3333333333333333703, 0.3333333333333333703, 0.3333333333333333703, 0.3333333333333333703, 0.3333333333333333703, 0.3333333333333333703, 0.3333333333333333703, 0.3333333333333333703, 0.3333333333333333703, 0.3333333333333333703, 0.3333333333333333703, 0.3333333333333333703, 0.3333333333333333703, 0.3333333333333333703, 0.3333333333333333703, 0.3333333333333333703, 0.3333333333333333703, 0.3333333333333333703, 0.3333333333333333703, 0.3333333333333333703, 0.3333333333333333703, 0.3333333333333333703, 0.3333333333333333703, 0.3333333333333333703, 0.3333333333333333703, 0.3333333333333333703, 0.3333333333333333703, 0.3333333333333333703, 0.3333333333333333703, 0.3333333333333333703, 0.3333333333333333703, 0.3333333333333333703, 0.3333333333333333703, 0.3333333333333333703, 0.3333333333333333703, 0.3333333333333333703, 0.3333333333333333703, 0.3333333333333333703, 0.3333333333333333703, 0.3333333333333333703, 0.3333333333333333703, 0.3333333333333333703, 0.3333333333333333703, 0.3333333333333333703, 0.3333333333333333703, 0.3333333333333333703, 0.3333333333333333703, 0.3333333333333333703, 0.3333333333333333703, 0.3333333333333333703, 0.3333333333333333703, 0.3333333333333333703, 0.3333333333333333703, 0.3333333333333333703, 0.3333333333333333703, 0.3333333333333333703, 0.3333333333333333703, 0.3333333333333333703, 0.3333333333333333703, 0.3333333333333333703, 0.3333333333333333703, 0.3333333333333333703, 0.3333333333333333703, 0.3333333333333333703, 0.3333333333333333703, 0.3333333333333333703, 0.3333333333333333703, 0.3333333333333333703, 0.3333333333333333703, 0.3333333333333333703, 0.3333333333333333703, 0.3333333333333333703, 0.3333333333333333703, 0.3333333333333333703, 0.3333333333333333703, 0.3333333333333333703, 0.3333333333333333703, 0.3333333333333333703, 0.3333333333333333703, 0.3333333333333333703, 0.3333333333333333703, 0.3333333333333333703, 0.3333333333333333703, 0.3333333333333333703, 0.3333333333333333703, 0.3333333333333333703, 0.3333333333333333703, 0.3333333333333333703, 0.3333333333333333703, 0.3333333333333333703, 0.3333333333333333703, 0.3333333333333333703, 0.3333333333333333703, 0.3333333333333333703, 0.3333333333333333703, 0.3333333333333333703, 0.3333333333333333703, 0.3333333333333333703, 0.3333333333333333703, 0.3333333333333333703, 0.3333333333333333703, 0.3333333333333333703, 0.3333333333333333703, 0.3333333333333333703, 0.3333333333333333703, 0.3333333333333333703, 0.3333333333333333703, 0.3333333333333333703, 0.3333333333333333703, 0.3333333333333333703, 0.3333333333333333703, 0.3333333333333333703, 0.3333333333333333703, 0.3333333333333333703, 0.3333333333333333703, 0.3333333333333333703, 0.3333333333333333703, 0.3333333333333333703, 0.3333333333333333703, 0.3333333333333333703, 0.3333333333333333703, 0.3333333333333333703, 0.3333333333333333703, 0.3333333333333333703, 0.3333333333333333703, 0.3333333333333333703, 0.3333333333333333703, 0.3333333333333333703, 0.3333333333333333703, 0.3333333333333333703, 0.3333333333333333703, 0.3333333333333333703, 0.3333333333333333703, 0.3333333333333333703, 0.3333333333333333703, 0.3333333333333333703, 0.3333333333333333703, 0.3333333333333333703, 0.3333333333333333703, 0.3333333333333333703, 0.3333333333333333703, 0.3333333333333333703, 0.3333333333333333703, 0.3333333333333333703, 0.3333333333333333703, 0.3333333333333333703, 0.3333333333333333703, 0.3333333333333333703, 0.3333333333333333703, 0.3333333333333333703, 0.3333333333333333703, 0.3333333333333333703, 0.3333333333333333703, 0.3333333333333333703, 0.3333333333333333703, 0.3333333333333333703, 0.3333333333333333703, 0.3333333333333333703, 0.3333333333333333703, 0.3333333333333333703, 0.3333333333333333703, 0.3333333333333333703, 0.3333333333333333703, 0.3333333333333333703, 0.3333333333333333703, 0.3333333333333333703, 0.3333333333333333703, 0.3333333333333333703, 0.3333333333333333703, 0.3333333333333333703, 0.3333333333333333703, 0.3333333333333333703, 0.3333333333333333703, 0.3333333333333333703, 0.3333333333333333703, 0.3333333333333333703, 0.3333333333333333703, 0.3333333333333333703, 0.3333333333333333703, 0.3333333333333333703, 0.3333333333333333703, 0.3333333333333333703, 0.3333333333333333703, 0.3333333333333333703, 0.3333333333333333703, 0.3333333333333333703, 0.3333333333333333703, 0.3333333333333333703, 0.3333333333333333703, 0.3333333333333333703),
 ( 1.000000000000000000, 1.000000000000000000, 1.000000000000000000, 1.000000000000000000, 1.000000000000000000, 1.000000000000000000, 1.000000000000000000, 1.000000000000000000, 1.000000000000000000, 1.000000000000000000, 1.000000000000000000, 1.000000000000000000, 1.000000000000000000, 1.000000000000000000, 1.000000000000000000, 1.000000000000000000, 1.000000000000000000, 1.000000000000000000, 1.000000000000000000, 1.000000000000000000, 1.000000000000000000, 1.000000000000000000, 1.000000000000000000, 1.000000000000000000, 1.000000000000000000, 1.000000000000000000, 1.000000000000000000, 1.000000000000000000, 1.000000000000000000, 1.000000000000000000, 1.000000000000000000, 1.000000000000000000, 1.000000000000000000, 1.000000000000000000, 1.000000000000000000, 1.000000000000000000, 1.000000000000000000, 1.000000000000000000, 1.000000000000000000, 1.000000000000000000, 1.000000000000000000, 1.000000000000000000, 1.000000000000000000, 1.000000000000000000, 1.000000000000000000, 1.000000000000000000, 1.000000000000000000, 1.000000000000000000, 1.000000000000000000, 1.000000000000000000, 1.000000000000000000, 1.000000000000000000, 1.000000000000000000, 1.000000000000000000, 1.000000000000000000, 1.000000000000000000, 1.000000000000000000, 1.000000000000000000, 1.000000000000000000, 1.000000000000000000, 1.000000000000000000, 1.000000000000000000, 1.000000000000000000, 1.000000000000000000, 1.000000000000000000, 1.000000000000000000, 1.000000000000000000, 1.000000000000000000, 1.000000000000000000, 1.000000000000000000, 1.000000000000000000, 1.000000000000000000, 1.000000000000000000, 1.000000000000000000, 1.000000000000000000, 1.000000000000000000, 1.000000000000000000, 1.000000000000000000, 1.000000000000000000, 1.000000000000000000, 1.000000000000000000, 1.000000000000000000, 1.000000000000000000, 1.000000000000000000, 1.000000000000000000, 1.000000000000000000, 1.000000000000000000, 1.000000000000000000, 1.000000000000000000, 1.000000000000000000, 1.000000000000000000, 1.000000000000000000, 1.000000000000000000, 1.000000000000000000, 1.000000000000000000, 1.000000000000000000, 1.000000000000000000, 1.000000000000000000, 1.000000000000000000, 1.000000000000000000, 1.000000000000000000, 1.000000000000000000, 1.000000000000000000, 1.000000000000000000, 1.000000000000000000, 1.000000000000000000, 1.000000000000000000, 1.000000000000000000, 1.000000000000000000, 1.000000000000000000, 1.000000000000000000, 1.000000000000000000, 1.000000000000000000, 1.000000000000000000, 1.000000000000000000, 1.000000000000000000, 1.000000000000000000, 1.000000000000000000, 1.000000000000000000, 1.000000000000000000, 1.000000000000000000, 1.000000000000000000, 1.000000000000000000, 1.000000000000000000, 1.000000000000000000, 1.000000000000000000, 1.000000000000000000, 1.000000000000000000, 1.000000000000000000, 1.000000000000000000, 1.000000000000000000, 1.000000000000000000, 1.000000000000000000, 1.000000000000000000, 1.000000000000000000, 1.000000000000000000, 1.000000000000000000, 1.000000000000000000, 1.000000000000000000, 1.000000000000000000, 1.000000000000000000, 1.000000000000000000, 1.000000000000000000, 1.000000000000000000, 1.000000000000000000, 1.000000000000000000, 1.000000000000000000, 1.000000000000000000, 1.000000000000000000, 1.000000000000000000, 1.000000000000000000, 1.000000000000000000, 1.000000000000000000, 1.000000000000000000, 1.000000000000000000, 1.000000000000000000, 1.000000000000000000, 1.000000000000000000, 1.000000000000000000, 1.000000000000000000, 1.000000000000000000, 1.000000000000000000, 1.000000000000000000, 1.000000000000000000, 1.000000000000000000, 1.000000000000000000, 1.000000000000000000, 1.000000000000000000, 1.000000000000000000, 1.000000000000000000, 1.000000000000000000, 1.000000000000000000, 1.000000000000000000, 1.000000000000000000, 1.000000000000000000, 1.000000000000000000, 1.000000000000000000, 1.000000000000000000, 1.000000000000000000, 1.000000000000000000, 1.000000000000000000, 1.000000000000000000, 1.000000000000000000, 1.000000000000000000, 1.000000000000000000, 1.000000000000000000, 1.000000000000000000, 1.000000000000000000, 1.000000000000000000, 1.000000000000000000, 1.000000000000000000, 1.000000000000000000, 1.000000000000000000, 1.000000000000000000, 1.000000000000000000, 1.000000000000000000, 1.000000000000000000, 1.000000000000000000, 1.000000000000000000, 1.000000000000000000, 1.000000000000000000, 1.000000000000000000, 1.000000000000000000, 1.000000000000000000, 1.000000000000000000, 1.000000000000000000, 1.000000000000000000, 1.000000000000000000, 1.000000000000000000, 1.000000000000000000, 1.000000000000000000, 1.000000000000000000, 1.000000000000000000, 1.000000000000000000, 1.000000000000000000, 1.000000000000000000, 1.000000000000000000, 1.000000000000000000, 1.000000000000000000, 1.000000000000000000, 1.000000000000000000, 1.000000000000000000, 1.000000000000000000, 1.000000000000000000, 1.000000000000000000, 1.000000000000000000, 1.000000000000000000, 1.000000000000000000, 1.000000000000000000, 1.000000000000000000, 1.000000000000000000, 1.000000000000000000, 1.000000000000000000, 1.000000000000000000, 1.000000000000000000, 1.000000000000000000, 1.000000000000000000, 1.000000000000000000, 1.000000000000000000, 1.000000000000000000, 1.000000000000000000, 1.000000000000000000, 1.000000000000000000, 1.000000000000000000, 1.000000000000000000, 1.000000000000000000, 1.000000000000000000, 1.000000000000000000, 1.000000000000000000, 1.000000000000000000, 1.000000000000000000, 1.000000000000000000, 1.000000000000000000, 1.000000000000000000, 1.000000000000000000, 1.000000000000000000, 1.000000000000000000, 1.000000000000000000, 1.000000000000000000, 1.000000000000000000, 1.000000000000000000, 1.000000000000000000, 1.000000000000000000, 1.000000000000000000, 1.000000000000000000, 1.000000000000000000, 1.000000000000000000, 1.000000000000000000, 1.000000000000000000, 1.000000000000000000, 1.000000000000000000, 1.000000000000000000, 1.000000000000000000, 1.000000000000000000, 1.000000000000000000, 1.000000000000000000, 1.000000000000000000, 1.000000000000000000, 1.000000000000000000, 1.000000000000000000, 1.000000000000000000, 1.000000000000000000, 1.000000000000000000, 1.000000000000000000, 1.000000000000000000, 1.000000000000000000, 1.000000000000000000, 1.000000000000000000, 1.000000000000000000, 1.000000000000000000, 1.000000000000000000, 1.000000000000000000, 1.000000000000000000, 1.000000000000000000, 1.000000000000000000, 1.000000000000000000, 1.000000000000000000, 1.000000000000000000, 1.000000000000000000, 1.000000000000000000, 1.000000000000000000, 1.000000000000000000, 1.000000000000000000, 1.000000000000000000, 1.000000000000000000, 1.000000000000000000, 1.000000000000000000, 1.000000000000000000, 1.000000000000000000, 1.000000000000000000, 1.000000000000000000, 1.000000000000000000, 1.000000000000000000, 1.000000000000000000, 1.000000000000000000, 1.000000000000000000, 1.000000000000000000, 1.000000000000000000, 1.000000000000000000, 1.000000000000000000, 1.000000000000000000, 1.000000000000000000, 1.000000000000000000, 1.000000000000000000, 1.000000000000000000, 1.000000000000000000, 1.000000000000000000, 1.000000000000000000, 1.000000000000000000, 1.000000000000000000, 1.000000000000000000, 1.000000000000000000, 1.000000000000000000, 1.000000000000000000, 1.000000000000000000, 1.000000000000000000),
 ( 0.3333333333333333703, 0.3333333333333333703, 0.3333333333333333703, 0.3333333333333333703, 0.3333333333333333703, 0.3333333333333333703, 0.3333333333333333703, 0.3333333333333333703, 0.3333333333333333703, 0.3333333333333333703, 0.3333333333333333703, 0.3333333333333333703, 0.3333333333333333703, 0.3333333333333333703, 0.3333333333333333703, 0.3333333333333333703, 0.3333333333333333703, 0.3333333333333333703, 0.3333333333333333703, 0.3333333333333333703, 0.3333333333333333703, 0.3333333333333333703, 0.3333333333333333703, 0.3333333333333333703, 0.3333333333333333703, 0.3333333333333333703, 0.3333333333333333703, 0.3333333333333333703, 0.3333333333333333703, 0.3333333333333333703, 0.3333333333333333703, 0.3333333333333333703, 0.3333333333333333703, 0.3333333333333333703, 0.3333333333333333703, 0.3333333333333333703, 0.3333333333333333703, 0.3333333333333333703, 0.3333333333333333703, 0.3333333333333333703, 0.3333333333333333703, 0.3333333333333333703, 0.3333333333333333703, 0.3333333333333333703, 0.3333333333333333703, 0.3333333333333333703, 0.3333333333333333703, 0.3333333333333333703, 0.3333333333333333703, 0.3333333333333333703, 0.3333333333333333703, 0.3333333333333333703, 0.3333333333333333703, 0.3333333333333333703, 0.3333333333333333703, 0.3333333333333333703, 0.3333333333333333703, 0.3333333333333333703, 0.3333333333333333703, 0.3333333333333333703, 0.3333333333333333703, 0.3333333333333333703, 0.3333333333333333703, 0.3333333333333333703, 0.3333333333333333703, 0.3333333333333333703, 0.3333333333333333703, 0.3333333333333333703, 0.3333333333333333703, 0.3333333333333333703, 0.3333333333333333703, 0.3333333333333333703, 0.3333333333333333703, 0.3333333333333333703, 0.3333333333333333703, 0.3333333333333333703, 0.3333333333333333703, 0.3333333333333333703, 0.3333333333333333703, 0.3333333333333333703, 0.3333333333333333703, 0.3333333333333333703, 0.3333333333333333703, 0.3333333333333333703, 0.3333333333333333703, 0.3333333333333333703, 0.3333333333333333703, 0.3333333333333333703, 0.3333333333333333703, 0.3333333333333333703, 0.3333333333333333703, 0.3333333333333333703, 0.3333333333333333703, 0.3333333333333333703, 0.3333333333333333703, 0.3333333333333333703, 0.3333333333333333703, 0.3333333333333333703, 0.3333333333333333703, 0.3333333333333333703, 0.3333333333333333703, 0.3333333333333333703, 0.3333333333333333703, 0.3333333333333333703, 0.3333333333333333703, 0.3333333333333333703, 0.3333333333333333703, 0.3333333333333333703, 0.3333333333333333703, 0.3333333333333333703, 0.3333333333333333703, 0.3333333333333333703, 0.3333333333333333703, 0.3333333333333333703, 0.3333333333333333703, 0.3333333333333333703, 0.3333333333333333703, 0.3333333333333333703, 0.3333333333333333703, 0.3333333333333333703, 0.3333333333333333703, 0.3333333333333333703, 0.3333333333333333703, 0.3333333333333333703, 0.3333333333333333703, 0.3333333333333333703, 0.3333333333333333703, 0.3333333333333333703, 0.3333333333333333703, 0.3333333333333333703, 0.3333333333333333703, 0.3333333333333333703, 0.3333333333333333703, 0.3333333333333333703, 0.3333333333333333703, 0.3333333333333333703, 0.3333333333333333703, 0.3333333333333333703, 0.3333333333333333703, 0.3333333333333333703, 0.3333333333333333703, 0.3333333333333333703, 0.3333333333333333703, 0.3333333333333333703, 0.3333333333333333703, 0.3333333333333333703, 0.3333333333333333703, 0.3333333333333333703, 0.3333333333333333703, 0.3333333333333333703, 0.3333333333333333703, 0.3333333333333333703, 0.3333333333333333703, 0.3333333333333333703, 0.3333333333333333703, 0.3333333333333333703, 0.3333333333333333703, 0.3333333333333333703, 0.3333333333333333703, 0.3333333333333333703, 0.3333333333333333703, 0.3333333333333333703, 0.3333333333333333703, 0.3333333333333333703, 0.3333333333333333703, 0.3333333333333333703, 0.3333333333333333703, 0.3333333333333333703, 0.3333333333333333703, 0.3333333333333333703, 0.3333333333333333703, 0.3333333333333333703, 0.3333333333333333703, 0.3333333333333333703, 0.3333333333333333703, 0.3333333333333333703, 0.3333333333333333703, 0.3333333333333333703, 0.3333333333333333703, 0.3333333333333333703, 0.3333333333333333703, 0.3333333333333333703, 0.3333333333333333703, 0.3333333333333333703, 0.3333333333333333703, 0.3333333333333333703, 0.3333333333333333703, 0.3333333333333333703, 0.3333333333333333703, 0.3333333333333333703, 0.3333333333333333703, 0.3333333333333333703, 0.3333333333333333703, 0.3333333333333333703, 0.3333333333333333703, 0.3333333333333333703, 0.3333333333333333703, 0.3333333333333333703, 0.3333333333333333703, 0.3333333333333333703, 0.3333333333333333703, 0.3333333333333333703, 0.3333333333333333703, 0.3333333333333333703, 0.3333333333333333703, 0.3333333333333333703, 0.3333333333333333703, 0.3333333333333333703, 0.3333333333333333703, 0.3333333333333333703, 0.3333333333333333703, 0.3333333333333333703, 0.3333333333333333703, 0.3333333333333333703, 0.3333333333333333703, 0.3333333333333333703, 0.3333333333333333703, 0.3333333333333333703, 0.3333333333333333703, 0.3333333333333333703, 0.3333333333333333703, 0.3333333333333333703, 0.3333333333333333703, 0.3333333333333333703, 0.3333333333333333703, 0.3333333333333333703, 0.3333333333333333703, 0.3333333333333333703, 0.3333333333333333703, 0.3333333333333333703, 0.3333333333333333703, 0.3333333333333333703, 0.3333333333333333703, 0.3333333333333333703, 0.3333333333333333703, 0.3333333333333333703, 0.3333333333333333703, 0.3333333333333333703, 0.3333333333333333703, 0.3333333333333333703, 0.3333333333333333703, 0.3333333333333333703, 0.3333333333333333703, 0.3333333333333333703, 0.3333333333333333703, 0.3333333333333333703, 0.3333333333333333703, 0.3333333333333333703, 0.3333333333333333703, 0.3333333333333333703, 0.3333333333333333703, 0.3333333333333333703, 0.3333333333333333703, 0.3333333333333333703, 0.3333333333333333703, 0.3333333333333333703, 0.3333333333333333703, 0.3333333333333333703, 0.3333333333333333703, 0.3333333333333333703, 0.3333333333333333703, 0.3333333333333333703, 0.3333333333333333703, 0.3333333333333333703, 0.3333333333333333703, 0.3333333333333333703, 0.3333333333333333703, 0.3333333333333333703, 0.3333333333333333703, 0.3333333333333333703, 0.3333333333333333703, 0.3333333333333333703, 0.3333333333333333703, 0.3333333333333333703, 0.3333333333333333703, 0.3333333333333333703, 0.3333333333333333703, 0.3333333333333333703, 0.3333333333333333703, 0.3333333333333333703, 0.3333333333333333703, 0.3333333333333333703, 0.3333333333333333703, 0.3333333333333333703, 0.3333333333333333703, 0.3333333333333333703, 0.3333333333333333703, 0.3333333333333333703, 0.3333333333333333703, 0.3333333333333333703, 0.3333333333333333703, 0.3333333333333333703, 0.3333333333333333703, 0.3333333333333333703, 0.3333333333333333703, 0.3333333333333333703, 0.3333333333333333703, 0.3333333333333333703, 0.3333333333333333703, 0.3333333333333333703, 0.3333333333333333703, 0.3333333333333333703, 0.3333333333333333703, 0.3333333333333333703, 0.3333333333333333703, 0.3333333333333333703, 0.3333333333333333703, 0.3333333333333333703, 0.3333333333333333703, 0.3333333333333333703, 0.3333333333333333703, 0.3333333333333333703, 0.3333333333333333703, 0.3333333333333333703, 0.3333333333333333703, 0.3333333333333333703, 0.3333333333333333703, 0.3333333333333333703, 0.3333333333333333703, 0.3333333333333333703, 0.3333333333333333703, 0.3333333333333333703, 0.3333333333333333703, 0.3333333333333333703, 0.3333333333333333703, 0.3333333333333333703, 0.3333333333333333703, 0.3333333333333333703, 0.3333333333333333703, 0.3333333333333333703, 0.3333333333333333703, 0.3333333333333333703, 0.3333333333333333703, 0.3333333333333333703, 0.3333333333333333703, 0.3333333333333333703),
 ( 0.3333333333333333703, 0.3333333333333333703, 0.3333333333333333703, 0.3333333333333333703, 0.3333333333333333703, 0.3333333333333333703, 0.3333333333333333703, 0.3333333333333333703, 0.3333333333333333703, 0.3333333333333333703, 0.3333333333333333703, 0.3333333333333333703, 0.3333333333333333703, 0.3333333333333333703, 0.3333333333333333703, 0.3333333333333333703, 0.3333333333333333703, 0.3333333333333333703, 0.3333333333333333703, 0.3333333333333333703, 0.3333333333333333703, 0.3333333333333333703, 0.3333333333333333703, 0.3333333333333333703, 0.3333333333333333703, 0.3333333333333333703, 0.3333333333333333703, 0.3333333333333333703, 0.3333333333333333703, 0.3333333333333333703, 0.3333333333333333703, 0.3333333333333333703, 0.3333333333333333703, 0.3333333333333333703, 0.3333333333333333703, 0.3333333333333333703, 0.3333333333333333703, 0.3333333333333333703, 0.3333333333333333703, 0.3333333333333333703, 0.3333333333333333703, 0.3333333333333333703, 0.3333333333333333703, 0.3333333333333333703, 0.3333333333333333703, 0.3333333333333333703, 0.3333333333333333703, 0.3333333333333333703, 0.3333333333333333703, 0.3333333333333333703, 0.3333333333333333703, 0.3333333333333333703, 0.3333333333333333703, 0.3333333333333333703, 0.3333333333333333703, 0.3333333333333333703, 0.3333333333333333703, 0.3333333333333333703, 0.3333333333333333703, 0.3333333333333333703, 0.3333333333333333703, 0.3333333333333333703, 0.3333333333333333703, 0.3333333333333333703, 0.3333333333333333703, 0.3333333333333333703, 0.3333333333333333703, 0.3333333333333333703, 0.3333333333333333703, 0.3333333333333333703, 0.3333333333333333703, 0.3333333333333333703, 0.3333333333333333703, 0.3333333333333333703, 0.3333333333333333703, 0.3333333333333333703, 0.3333333333333333703, 0.3333333333333333703, 0.3333333333333333703, 0.3333333333333333703, 0.3333333333333333703, 0.3333333333333333703, 0.3333333333333333703, 0.3333333333333333703, 0.3333333333333333703, 0.3333333333333333703, 0.3333333333333333703, 0.3333333333333333703, 0.3333333333333333703, 0.3333333333333333703, 0.3333333333333333703, 0.3333333333333333703, 0.3333333333333333703, 0.3333333333333333703, 0.3333333333333333703, 0.3333333333333333703, 0.3333333333333333703, 0.3333333333333333703, 0.3333333333333333703, 0.3333333333333333703, 0.3333333333333333703, 0.3333333333333333703, 0.3333333333333333703, 0.3333333333333333703, 0.3333333333333333703, 0.3333333333333333703, 0.3333333333333333703, 0.3333333333333333703, 0.3333333333333333703, 0.3333333333333333703, 0.3333333333333333703, 0.3333333333333333703, 0.3333333333333333703, 0.3333333333333333703, 0.3333333333333333703, 0.3333333333333333703, 0.3333333333333333703, 0.3333333333333333703, 0.3333333333333333703, 0.3333333333333333703, 0.3333333333333333703, 0.3333333333333333703, 0.3333333333333333703, 0.3333333333333333703, 0.3333333333333333703, 0.3333333333333333703, 0.3333333333333333703, 0.3333333333333333703, 0.3333333333333333703, 0.3333333333333333703, 0.3333333333333333703, 0.3333333333333333703, 0.3333333333333333703, 0.3333333333333333703, 0.3333333333333333703, 0.3333333333333333703, 0.3333333333333333703, 0.3333333333333333703, 0.3333333333333333703, 0.3333333333333333703, 0.3333333333333333703, 0.3333333333333333703, 0.3333333333333333703, 0.3333333333333333703, 0.3333333333333333703, 0.3333333333333333703, 0.3333333333333333703, 0.3333333333333333703, 0.3333333333333333703, 0.3333333333333333703, 0.3333333333333333703, 0.3333333333333333703, 0.3333333333333333703, 0.3333333333333333703, 0.3333333333333333703, 0.3333333333333333703, 0.3333333333333333703, 0.3333333333333333703, 0.3333333333333333703, 0.3333333333333333703, 0.3333333333333333703, 0.3333333333333333703, 0.3333333333333333703, 0.3333333333333333703, 0.3333333333333333703, 0.3333333333333333703, 0.3333333333333333703, 0.3333333333333333703, 0.3333333333333333703, 0.3333333333333333703, 0.3333333333333333703, 0.3333333333333333703, 0.3333333333333333703, 0.3333333333333333703, 0.3333333333333333703, 0.3333333333333333703, 0.3333333333333333703, 0.3333333333333333703, 0.3333333333333333703, 0.3333333333333333703, 0.3333333333333333703, 0.3333333333333333703, 0.3333333333333333703, 0.3333333333333333703, 0.3333333333333333703, 0.3333333333333333703, 0.3333333333333333703, 0.3333333333333333703, 0.3333333333333333703, 0.3333333333333333703, 0.3333333333333333703, 0.3333333333333333703, 0.3333333333333333703, 0.3333333333333333703, 0.3333333333333333703, 0.3333333333333333703, 0.3333333333333333703, 0.3333333333333333703, 0.3333333333333333703, 0.3333333333333333703, 0.3333333333333333703, 0.3333333333333333703, 0.3333333333333333703, 0.3333333333333333703, 0.3333333333333333703, 0.3333333333333333703, 0.3333333333333333703, 0.3333333333333333703, 0.3333333333333333703, 0.3333333333333333703, 0.3333333333333333703, 0.3333333333333333703, 0.3333333333333333703, 0.3333333333333333703, 0.3333333333333333703, 0.3333333333333333703, 0.3333333333333333703, 0.3333333333333333703, 0.3333333333333333703, 0.3333333333333333703, 0.3333333333333333703, 0.3333333333333333703, 0.3333333333333333703, 0.3333333333333333703, 0.3333333333333333703, 0.3333333333333333703, 0.3333333333333333703, 0.3333333333333333703, 0.3333333333333333703, 0.3333333333333333703, 0.3333333333333333703, 0.3333333333333333703, 0.3333333333333333703, 0.3333333333333333703, 0.3333333333333333703, 0.3333333333333333703, 0.3333333333333333703, 0.3333333333333333703, 0.3333333333333333703, 0.3333333333333333703, 0.3333333333333333703, 0.3333333333333333703, 0.3333333333333333703, 0.3333333333333333703, 0.3333333333333333703, 0.3333333333333333703, 0.3333333333333333703, 0.3333333333333333703, 0.3333333333333333703, 0.3333333333333333703, 0.3333333333333333703, 0.3333333333333333703, 0.3333333333333333703, 0.3333333333333333703, 0.3333333333333333703, 0.3333333333333333703, 0.3333333333333333703, 0.3333333333333333703, 0.3333333333333333703, 0.3333333333333333703, 0.3333333333333333703, 0.3333333333333333703, 0.3333333333333333703, 0.3333333333333333703, 0.3333333333333333703, 0.3333333333333333703, 0.3333333333333333703, 0.3333333333333333703, 0.3333333333333333703, 0.3333333333333333703, 0.3333333333333333703, 0.3333333333333333703, 0.3333333333333333703, 0.3333333333333333703, 0.3333333333333333703, 0.3333333333333333703, 0.3333333333333333703, 0.3333333333333333703, 0.3333333333333333703, 0.3333333333333333703, 0.3333333333333333703, 0.3333333333333333703, 0.3333333333333333703, 0.3333333333333333703, 0.3333333333333333703, 0.3333333333333333703, 0.3333333333333333703, 0.3333333333333333703, 0.3333333333333333703, 0.3333333333333333703, 0.3333333333333333703, 0.3333333333333333703, 0.3333333333333333703, 0.3333333333333333703, 0.3333333333333333703, 0.3333333333333333703, 0.3333333333333333703, 0.3333333333333333703, 0.3333333333333333703, 0.3333333333333333703, 0.3333333333333333703, 0.3333333333333333703, 0.3333333333333333703, 0.3333333333333333703, 0.3333333333333333703, 0.3333333333333333703, 0.3333333333333333703, 0.3333333333333333703, 0.3333333333333333703, 0.3333333333333333703, 0.3333333333333333703, 0.3333333333333333703, 0.3333333333333333703, 0.3333333333333333703, 0.3333333333333333703, 0.3333333333333333703, 0.3333333333333333703, 0.3333333333333333703, 0.3333333333333333703, 0.3333333333333333703, 0.3333333333333333703, 0.3333333333333333703, 0.3333333333333333703, 0.3333333333333333703, 0.3333333333333333703, 0.3333333333333333703, 0.3333333333333333703, 0.3333333333333333703, 0.3333333333333333703, 0.3333333333333333703, 0.3333333333333333703, 0.3333333333333333703, 0.3333333333333333703, 0.3333333333333333703, 0.3333333333333333703, 0.3333333333333333703),
 ( 1.000000000000000000, 1.000000000000000000, 1.000000000000000000, 1.000000000000000000, 1.000000000000000000, 1.000000000000000000, 1.000000000000000000, 1.000000000000000000, 1.000000000000000000, 1.000000000000000000, 1.000000000000000000, 1.000000000000000000, 1.000000000000000000, 1.000000000000000000, 1.000000000000000000, 1.000000000000000000, 1.000000000000000000, 1.000000000000000000, 1.000000000000000000, 1.000000000000000000, 1.000000000000000000, 1.000000000000000000, 1.000000000000000000, 1.000000000000000000, 1.000000000000000000, 1.000000000000000000, 1.000000000000000000, 1.000000000000000000, 1.000000000000000000, 1.000000000000000000, 1.000000000000000000, 1.000000000000000000, 1.000000000000000000, 1.000000000000000000, 1.000000000000000000, 1.000000000000000000, 1.000000000000000000, 1.000000000000000000, 1.000000000000000000, 1.000000000000000000, 1.000000000000000000, 1.000000000000000000, 1.000000000000000000, 1.000000000000000000, 1.000000000000000000, 1.000000000000000000, 1.000000000000000000, 1.000000000000000000, 1.000000000000000000, 1.000000000000000000, 1.000000000000000000, 1.000000000000000000, 1.000000000000000000, 1.000000000000000000, 1.000000000000000000, 1.000000000000000000, 1.000000000000000000, 1.000000000000000000, 1.000000000000000000, 1.000000000000000000, 1.000000000000000000, 1.000000000000000000, 1.000000000000000000, 1.000000000000000000, 1.000000000000000000, 1.000000000000000000, 1.000000000000000000, 1.000000000000000000, 1.000000000000000000, 1.000000000000000000, 1.000000000000000000, 1.000000000000000000, 1.000000000000000000, 1.000000000000000000, 1.000000000000000000, 1.000000000000000000, 1.000000000000000000, 1.000000000000000000, 1.000000000000000000, 1.000000000000000000, 1.000000000000000000, 1.000000000000000000, 1.000000000000000000, 1.000000000000000000, 1.000000000000000000, 1.000000000000000000, 1.000000000000000000, 1.000000000000000000, 1.000000000000000000, 1.000000000000000000, 1.000000000000000000, 1.000000000000000000, 1.000000000000000000, 1.000000000000000000, 1.000000000000000000, 1.000000000000000000, 1.000000000000000000, 1.000000000000000000, 1.000000000000000000, 1.000000000000000000, 1.000000000000000000, 1.000000000000000000, 1.000000000000000000, 1.000000000000000000, 1.000000000000000000, 1.000000000000000000, 1.000000000000000000, 1.000000000000000000, 1.000000000000000000, 1.000000000000000000, 1.000000000000000000, 1.000000000000000000, 1.000000000000000000, 1.000000000000000000, 1.000000000000000000, 1.000000000000000000, 1.000000000000000000, 1.000000000000000000, 1.000000000000000000, 1.000000000000000000, 1.000000000000000000, 1.000000000000000000, 1.000000000000000000, 1.000000000000000000, 1.000000000000000000, 1.000000000000000000, 1.000000000000000000, 1.000000000000000000, 1.000000000000000000, 1.000000000000000000, 1.000000000000000000, 1.000000000000000000, 1.000000000000000000, 1.000000000000000000, 1.000000000000000000, 1.000000000000000000, 1.000000000000000000, 1.000000000000000000, 1.000000000000000000, 1.000000000000000000, 1.000000000000000000, 1.000000000000000000, 1.000000000000000000, 1.000000000000000000, 1.000000000000000000, 1.000000000000000000, 1.000000000000000000, 1.000000000000000000, 1.000000000000000000, 1.000000000000000000, 1.000000000000000000, 1.000000000000000000, 1.000000000000000000, 1.000000000000000000, 1.000000000000000000, 1.000000000000000000, 1.000000000000000000, 1.000000000000000000, 1.000000000000000000, 1.000000000000000000, 1.000000000000000000, 1.000000000000000000, 1.000000000000000000, 1.000000000000000000, 1.000000000000000000, 1.000000000000000000, 1.000000000000000000, 1.000000000000000000, 1.000000000000000000, 1.000000000000000000, 1.000000000000000000, 1.000000000000000000, 1.000000000000000000, 1.000000000000000000, 1.000000000000000000, 1.000000000000000000, 1.000000000000000000, 1.000000000000000000, 1.000000000000000000, 1.000000000000000000, 1.000000000000000000, 1.000000000000000000, 1.000000000000000000, 1.000000000000000000, 1.000000000000000000, 1.000000000000000000, 1.000000000000000000, 1.000000000000000000, 1.000000000000000000, 1.000000000000000000, 1.000000000000000000, 1.000000000000000000, 1.000000000000000000, 1.000000000000000000, 1.000000000000000000, 1.000000000000000000, 1.000000000000000000, 1.000000000000000000, 1.000000000000000000, 1.000000000000000000, 1.000000000000000000, 1.000000000000000000, 1.000000000000000000, 1.000000000000000000, 1.000000000000000000, 1.000000000000000000, 1.000000000000000000, 1.000000000000000000, 1.000000000000000000, 1.000000000000000000, 1.000000000000000000, 1.000000000000000000, 1.000000000000000000, 1.000000000000000000, 1.000000000000000000, 1.000000000000000000, 1.000000000000000000, 1.000000000000000000, 1.000000000000000000, 1.000000000000000000, 1.000000000000000000, 1.000000000000000000, 1.000000000000000000, 1.000000000000000000, 1.000000000000000000, 1.000000000000000000, 1.000000000000000000, 1.000000000000000000, 1.000000000000000000, 1.000000000000000000, 1.000000000000000000, 1.000000000000000000, 1.000000000000000000, 1.000000000000000000, 1.000000000000000000, 1.000000000000000000, 1.000000000000000000, 1.000000000000000000, 1.000000000000000000, 1.000000000000000000, 1.000000000000000000, 1.000000000000000000, 1.000000000000000000, 1.000000000000000000, 1.000000000000000000, 1.000000000000000000, 1.000000000000000000, 1.000000000000000000, 1.000000000000000000, 1.000000000000000000, 1.000000000000000000, 1.000000000000000000, 1.000000000000000000, 1.000000000000000000, 1.000000000000000000, 1.000000000000000000, 1.000000000000000000, 1.000000000000000000, 1.000000000000000000, 1.000000000000000000, 1.000000000000000000, 1.000000000000000000, 1.000000000000000000, 1.000000000000000000, 1.000000000000000000, 1.000000000000000000, 1.000000000000000000, 1.000000000000000000, 1.000000000000000000, 1.000000000000000000, 1.000000000000000000, 1.000000000000000000, 1.000000000000000000, 1.000000000000000000, 1.000000000000000000, 1.000000000000000000, 1.000000000000000000, 1.000000000000000000, 1.000000000000000000, 1.000000000000000000, 1.000000000000000000, 1.000000000000000000, 1.000000000000000000, 1.000000000000000000, 1.000000000000000000, 1.000000000000000000, 1.000000000000000000, 1.000000000000000000, 1.000000000000000000, 1.000000000000000000, 1.000000000000000000, 1.000000000000000000, 1.000000000000000000, 1.000000000000000000, 1.000000000000000000, 1.000000000000000000, 1.000000000000000000, 1.000000000000000000, 1.000000000000000000, 1.000000000000000000, 1.000000000000000000, 1.000000000000000000, 1.000000000000000000, 1.000000000000000000, 1.000000000000000000, 1.000000000000000000, 1.000000000000000000, 1.000000000000000000, 1.000000000000000000, 1.000000000000000000, 1.000000000000000000, 1.000000000000000000, 1.000000000000000000, 1.000000000000000000, 1.000000000000000000, 1.000000000000000000, 1.000000000000000000, 1.000000000000000000, 1.000000000000000000, 1.000000000000000000, 1.000000000000000000, 1.000000000000000000, 1.000000000000000000, 1.000000000000000000, 1.000000000000000000, 1.000000000000000000, 1.000000000000000000, 1.000000000000000000, 1.000000000000000000, 1.000000000000000000, 1.000000000000000000, 1.000000000000000000, 1.000000000000000000, 1.000000000000000000, 1.000000000000000000, 1.000000000000000000) ) ) 
 REPRESENTATION_ITEM ( '' )  SURFACE ( )  );
#12331 = TOROIDAL_SURFACE ( 'NONE', #8025, 24.63401512838747820, 3.000000000000000888 ) ;
#12332 = CARTESIAN_POINT ( 'NONE',  ( 10.03842945413050458, 28.43460431997513638, -225.8374938385031214 ) ) ;
#12333 = CARTESIAN_POINT ( 'NONE',  ( 15.39025625686376841, 1.044190007782545226, -218.9203249718910911 ) ) ;
#12334 = CARTESIAN_POINT ( 'NONE',  ( 11.75404126451729070, 5.688294280104953415, -229.3533586468489602 ) ) ;
#12335 = CARTESIAN_POINT ( 'NONE',  ( 16.43596176044053081, -17.06621466254232544, -232.8418678805942648 ) ) ;
#12336 = CARTESIAN_POINT ( 'NONE',  ( 0.000000000000000000, -23.00000000000006040, 75.00000000000000000 ) ) ;
#12337 = DIRECTION ( 'NONE',  ( -1.000000000000000000, 0.000000000000000000, 0.000000000000000000 ) ) ;
#12338 = CARTESIAN_POINT ( 'NONE',  ( -6.855867220396999251, 12.17758473459128332, -220.6375607554995213 ) ) ;
#12339 = CARTESIAN_POINT ( 'NONE',  ( 23.20431681157275605, -3.694239143335118492, -219.1264243754107781 ) ) ;
#12340 = CARTESIAN_POINT ( 'NONE',  ( 14.96415947227435339, -1.927366939720012606, -222.7010313878448358 ) ) ;
#12341 = CARTESIAN_POINT ( 'NONE',  ( 20.89184612657454920, 5.404957034965973683, -232.0952743654565609 ) ) ;
#12342 = CARTESIAN_POINT ( 'NONE',  ( -25.61997837663875188, 10.01664178086244483, -231.6711741719404074 ) ) ;
#12343 = CARTESIAN_POINT ( 'NONE',  ( 1.904360901363437275, -12.77109371939166138, -224.5066922355585177 ) ) ;
#12344 = DIRECTION ( 'NONE',  ( 1.000000000000000000, 0.000000000000000000, 0.000000000000000000 ) ) ;
#12345 = CARTESIAN_POINT ( 'NONE',  ( -23.98802705797876200, 19.46654170242919690, -223.5293093576406989 ) ) ;
#12347 = CARTESIAN_POINT ( 'NONE',  ( -22.57859951143173660, 16.82392524473188899, -219.5628058978911383 ) ) ;
#12346 = AXIS2_PLACEMENT_3D ( 'NONE', #9158, #7247, #16127 ) ;
#12348 = ORIENTED_EDGE ( 'NONE', *, *, #10673, .T. ) ;
#12349 = CARTESIAN_POINT ( 'NONE',  ( -15.23434562258889891, -0.4010941804143903222, -220.4743703065900036 ) ) ;
#12350 = CARTESIAN_POINT ( 'NONE',  ( -19.18273340400098448, -14.85130345181434741, -232.7114379411565039 ) ) ;
#12351 = CIRCLE ( 'NONE', #16300, 3.000000000000002665 ) ;
#12352 = CARTESIAN_POINT ( 'NONE',  ( -1.232595164407830946E-29, 17.50000000000007105, -24.99999999999999645 ) ) ;
#12353 = DIRECTION ( 'NONE',  ( -1.224646799147353207E-16, 1.000000000000000000, 3.540705920434612608E-33 ) ) ;
#12354 = CARTESIAN_POINT ( 'NONE',  ( -13.55591840520136770, 8.363404288414606924, -231.2690188357804857 ) ) ;
#12355 = CARTESIAN_POINT ( 'NONE',  ( 0.6837842112036801590, -24.48318360891119028, -216.1006322475167281 ) ) ;
#12356 = DIRECTION ( 'NONE',  ( -0.000000000000000000, -0.000000000000000000, -1.000000000000000000 ) ) ;
#12357 = CARTESIAN_POINT ( 'NONE',  ( 18.77038210872051849, -2.992569296362960873, -225.2431827457303655 ) ) ;
#12358 = CARTESIAN_POINT ( 'NONE',  ( 24.52860916307685457, 12.75391509163817361, -221.3604763108436941 ) ) ;
#12359 = CARTESIAN_POINT ( 'NONE',  ( -4.591517861330576267, 12.55780501983563191, -223.5932882008353033 ) ) ;
#12360 = CARTESIAN_POINT ( 'NONE',  ( -16.02266676603872142, 0.000000000000000000, -100.7764571353075524 ) ) ;
#12361 = CARTESIAN_POINT ( 'NONE',  ( 18.51425713624010427, 11.82474821235740592, -231.3645840199355632 ) ) ;
#12362 = CARTESIAN_POINT ( 'NONE',  ( 3.520698644836853131, -14.14291361662535884, -221.2714412251625618 ) ) ;
#12363 = ORIENTED_EDGE ( 'NONE', *, *, #20036, .T. ) ;
#12364 = CARTESIAN_POINT ( 'NONE',  ( -4.742143146070755932, 15.01230778631049567, -221.4832709320255049 ) ) ;
#12365 = PRODUCT_RELATED_PRODUCT_CATEGORY ( 'part', '', ( #20542 ) ) ;
#12366 = CARTESIAN_POINT ( 'NONE',  ( -15.82036597035495795, 4.920771916499852239, -223.0095317795067160 ) ) ;
#12367 = CARTESIAN_POINT ( 'NONE',  ( -27.05172747931452903, 14.36075930490012276, -228.5082213655825853 ) ) ;
#12368 = CARTESIAN_POINT ( 'NONE',  ( -12.19937816677273013, -10.70901586236097636, -226.3808855409166370 ) ) ;
#12369 = CARTESIAN_POINT ( 'NONE',  ( 0.000000000000000000, 0.000000000000000000, -30.00000000000000000 ) ) ;
#12370 = AXIS2_PLACEMENT_3D ( 'NONE', #14841, #17890, #9444 ) ;
#12371 = VERTEX_POINT ( 'NONE', #11128 ) ;
#12372 = CARTESIAN_POINT ( 'NONE',  ( 21.14328650935969023, 6.072767611243683916, -217.6422864096696514 ) ) ;
#12373 = CARTESIAN_POINT ( 'NONE',  ( 1.672997396509183110, -28.78979777605457713, -223.2908548649682814 ) ) ;
#12374 = CARTESIAN_POINT ( 'NONE',  ( 17.43816562714825125, 15.15720016074785903, -232.3748236813696906 ) ) ;
#12375 = CARTESIAN_POINT ( 'NONE',  ( -11.26857159993117996, 28.96895336474501192, -225.6039696848669678 ) ) ;
#12376 = CARTESIAN_POINT ( 'NONE',  ( 14.96462366732929716, 7.179279272144128754, -233.2042342402542374 ) ) ;
#12377 = CARTESIAN_POINT ( 'NONE',  ( 10.66614775643814994, 26.29080367171353672, -230.0818785118670178 ) ) ;
#12378 = CARTESIAN_POINT ( 'NONE',  ( -7.580942749559346439, 7.647666590413454202, 92.00000000000000000 ) ) ;
#12379 = CARTESIAN_POINT ( 'NONE',  ( -15.17658589853145479, -26.64966442869902252, -226.8090782225333442 ) ) ;
#12380 = CARTESIAN_POINT ( 'NONE',  ( 10.24538335401965661, -11.82980241027587276, -219.3753974371782363 ) ) ;
#12381 = CARTESIAN_POINT ( 'NONE',  ( 25.50000000000000000, 4.399999999999999467, -3.300000000000000266 ) ) ;
#12382 = VECTOR ( 'NONE', #16828, 1000.000000000000000 ) ;
#12383 = DIRECTION ( 'NONE',  ( 0.000000000000000000, 0.000000000000000000, 1.000000000000000000 ) ) ;
#12384 = CARTESIAN_POINT ( 'NONE',  ( -23.16143087541734502, 21.36835206473086046, -221.8715256527013651 ) ) ;
#12385 = CARTESIAN_POINT ( 'NONE',  ( -25.18517655442826353, -3.313270981248286340, -229.9274946033256697 ) ) ;
#12386 = CARTESIAN_POINT ( 'NONE',  ( 22.16327814861754675, 7.634676377199016706, -234.0520676664821735 ) ) ;
#12387 = CARTESIAN_POINT ( 'NONE',  ( 2.893760225568064115, 14.39521026618305477, -227.6654023557511550 ) ) ;
#12388 = CARTESIAN_POINT ( 'NONE',  ( 5.079647427451626562, 16.77877517420371234, -220.7769382327915366 ) ) ;
#12389 = ORIENTED_EDGE ( 'NONE', *, *, #8587, .T. ) ;
#12390 = CARTESIAN_POINT ( 'NONE',  ( 8.477993572791891808, -8.340333012420144243, -224.9486226631276793 ) ) ;
#12391 = VERTEX_POINT ( 'NONE', #19772 ) ;
#12392 = CARTESIAN_POINT ( 'NONE',  ( 21.39553407250273054, 8.453402029343234148, -217.9531594780983141 ) ) ;
#12393 = CARTESIAN_POINT ( 'NONE',  ( -10.33514150881494942, 13.62639309082336503, -216.9544063991933172 ) ) ;
#12394 = CARTESIAN_POINT ( 'NONE',  ( -15.54392142943450317, 6.670312097614393920, -219.6934017696036676 ) ) ;
#12395 = CARTESIAN_POINT ( 'NONE',  ( -17.66047203424674450, -3.377913611064220056, -232.7782090104293786 ) ) ;
#12396 = CARTESIAN_POINT ( 'NONE',  ( -20.18153419852512442, 14.25141268122526483, -233.5059133483111964 ) ) ;
#12397 = DIRECTION ( 'NONE',  ( 0.000000000000000000, 0.000000000000000000, 1.000000000000000000 ) ) ;
#12398 = CYLINDRICAL_SURFACE ( 'NONE', #19604, 2.000000000000000000 ) ;
#12399 =( GEOMETRIC_REPRESENTATION_CONTEXT ( 3 ) GLOBAL_UNCERTAINTY_ASSIGNED_CONTEXT ( ( #2668 ) ) GLOBAL_UNIT_ASSIGNED_CONTEXT ( ( #5436, #11985, #19173 ) ) REPRESENTATION_CONTEXT ( 'NONE', 'WORKASPACE' ) );
#12400 = CARTESIAN_POINT ( 'NONE',  ( -11.79656379827575918, 10.43402410864828589, -226.0519616335988076 ) ) ;
#12401 = CARTESIAN_POINT ( 'NONE',  ( 9.616550234602936342, 9.263684773868845923, -230.4827401731016607 ) ) ;
#12402 = CARTESIAN_POINT ( 'NONE',  ( 27.50364976068844669, 3.973406265104437729, -228.8805639113908228 ) ) ;
#12403 = EDGE_CURVE ( 'NONE', #22262, #6969, #17043, .T. ) ;
#12404 = CARTESIAN_POINT ( 'NONE',  ( -26.63259355655987548, -7.256793811979244779, -216.2488627322786101 ) ) ;
#12405 = CARTESIAN_POINT ( 'NONE',  ( -21.14773328851117995, -13.15959238732831693, -217.2646803791660943 ) ) ;
#12406 = CARTESIAN_POINT ( 'NONE',  ( -10.49339404011726984, 12.66576824096800991, -217.2681947942554643 ) ) ;
#12407 = CARTESIAN_POINT ( 'NONE',  ( -1.308474130992312023, -24.58654860180777391, -216.2430112183533026 ) ) ;
#12408 = CARTESIAN_POINT ( 'NONE',  ( 13.43170911749896490, 19.07691563292472026, -232.7497845103644636 ) ) ;
#12409 = CARTESIAN_POINT ( 'NONE',  ( 4.772350409791505932, -16.13531085440822466, -233.6884202312745344 ) ) ;
#12410 = FACE_OUTER_BOUND ( 'NONE', #20453, .T. ) ;
#12411 = CARTESIAN_POINT ( 'NONE',  ( -14.94640692938030746, 5.382918922058764544, -220.5478552936960455 ) ) ;
#12412 = FILL_AREA_STYLE ('',( #14109 ) ) ;
#12413 = CARTESIAN_POINT ( 'NONE',  ( -2.543684969149407227, 16.28137730373167713, -227.6987697727321915 ) ) ;
#12414 = CARTESIAN_POINT ( 'NONE',  ( -26.02492405343843984, 6.940268742526972900, -218.8798307745116460 ) ) ;
#12415 = CARTESIAN_POINT ( 'NONE',  ( 27.75679124201660741, 4.911524026080384075, -221.4430403652340829 ) ) ;
#12416 = CARTESIAN_POINT ( 'NONE',  ( 19.13999328532042910, 9.776920959053244431, -216.1190985676915375 ) ) ;
#12417 = CARTESIAN_POINT ( 'NONE',  ( -10.64756522805915395, -11.91724881161430361, -221.7317784521105750 ) ) ;
#12418 = AXIS2_PLACEMENT_3D ( 'NONE', #22265, #6868, #11593 ) ;
#12419 = MECHANICAL_DESIGN_GEOMETRIC_PRESENTATION_REPRESENTATION (  '', ( #17096 ), #12063 ) ;
#12420 = CARTESIAN_POINT ( 'NONE',  ( 18.15173157547545557, 23.32481284044927961, -217.8532150843729482 ) ) ;
#12421 = DIRECTION ( 'NONE',  ( -1.000000000000000000, 0.000000000000000000, 0.000000000000000000 ) ) ;
#12422 = CARTESIAN_POINT ( 'NONE',  ( -10.19343904566850867, -16.03376756945627335, -215.1857286610140250 ) ) ;
#12423 = CARTESIAN_POINT ( 'NONE',  ( -7.250603130619442283, 20.89725557392719324, -217.7893896917081520 ) ) ;
#12424 = CARTESIAN_POINT ( 'NONE',  ( 9.774133712851615030, 11.09751083462123766, -229.6876724410067823 ) ) ;
#12425 = CARTESIAN_POINT ( 'NONE',  ( -20.21481434941064848, 7.972326285609216967, -230.8475376972877484 ) ) ;
#12426 = CARTESIAN_POINT ( 'NONE',  ( -13.31245686955614005, 26.96290519511623174, -230.1796856776773836 ) ) ;
#12427 = CARTESIAN_POINT ( 'NONE',  ( 15.21408433160105034, 3.021350230896802103, -222.3056493717910769 ) ) ;
#12428 = ORIENTED_EDGE ( 'NONE', *, *, #13361, .T. ) ;
#12429 = EDGE_CURVE ( 'NONE', #8350, #3873, #12009, .T. ) ;
#12430 = CARTESIAN_POINT ( 'NONE',  ( 9.379155480182538085, -13.23755613463586300, -225.9392943819708250 ) ) ;
#12431 = AXIS2_PLACEMENT_3D ( 'NONE', #693, #2156, #5645 ) ;
#12432 = VERTEX_POINT ( 'NONE', #16305 ) ;
#12433 = CARTESIAN_POINT ( 'NONE',  ( 7.045253012492558753, -17.38872841331140862, -218.3726031779064556 ) ) ;
#12434 = CARTESIAN_POINT ( 'NONE',  ( -1.158668551263366986, 23.31492692626720853, -219.2372600964201865 ) ) ;
#12435 = PRESENTATION_STYLE_ASSIGNMENT (( #168 ) ) ;
#12436 = CARTESIAN_POINT ( 'NONE',  ( 8.496844655769807630, 14.66037471857024599, -219.1631158796573118 ) ) ;
#12437 = CARTESIAN_POINT ( 'NONE',  ( 24.59129902578158067, -8.191391589517788674, -218.4338547727923299 ) ) ;
#12438 = CARTESIAN_POINT ( 'NONE',  ( -20.83683780809167629, -19.66850649927503625, -219.7460615899071570 ) ) ;
#12439 = CARTESIAN_POINT ( 'NONE',  ( -5.178973235464019886, -24.35492185057628944, -233.6431870320687381 ) ) ;
#12440 = AXIS2_PLACEMENT_3D ( 'NONE', #9102, #434, #10893 ) ;
#12441 = CARTESIAN_POINT ( 'NONE',  ( -2.618694198633108261, 15.69630225547860825, -226.1451761977223498 ) ) ;
#12442 = DIRECTION ( 'NONE',  ( 1.000000000000000000, 0.000000000000000000, 0.000000000000000000 ) ) ;
#12443 = CARTESIAN_POINT ( 'NONE',  ( 24.38255093784924199, 7.851200578213498815, -231.2687759850219607 ) ) ;
#12444 = CARTESIAN_POINT ( 'NONE',  ( -16.39453490553961856, 20.24836633112041184, -233.1722131570092245 ) ) ;
#12445 = CARTESIAN_POINT ( 'NONE',  ( -2.723069588102707606, 15.58614045890443833, -225.0254611642426141 ) ) ;
#12446 = CARTESIAN_POINT ( 'NONE',  ( 0.1556102272723409452, 19.71550568250159685, -232.1993058477363547 ) ) ;
#12447 = CARTESIAN_POINT ( 'NONE',  ( -20.86570240061152148, 1.122719768445835875, -219.0984131021933763 ) ) ;
#12448 = CARTESIAN_POINT ( 'NONE',  ( 13.21888801141564151, 2.135177519634172238, -228.0426311217386797 ) ) ;
#12449 = EDGE_CURVE ( 'NONE', #945, #930, #14884, .T. ) ;
#12450 = CARTESIAN_POINT ( 'NONE',  ( 7.074707374710634156, -26.72731565888815553, -229.5909540767539738 ) ) ;
#12452 = CARTESIAN_POINT ( 'NONE',  ( 0.000000000000000000, 0.000000000000000000, 77.51594804401857175 ) ) ;
#12451 = AXIS2_PLACEMENT_3D ( 'NONE', #15898, #7352, #21054 ) ;
#12453 = VERTEX_POINT ( 'NONE', #14406 ) ;
#12454 =( GEOMETRIC_REPRESENTATION_CONTEXT ( 3 ) GLOBAL_UNCERTAINTY_ASSIGNED_CONTEXT ( ( #11452 ) ) GLOBAL_UNIT_ASSIGNED_CONTEXT ( ( #17010, #8234, #4840 ) ) REPRESENTATION_CONTEXT ( 'NONE', 'WORKASPACE' ) );
#12455 = CARTESIAN_POINT ( 'NONE',  ( 5.069241901512100412, 14.34986542013820632, -229.6420000777802954 ) ) ;
#12456 = CARTESIAN_POINT ( 'NONE',  ( 24.99579664921074240, -7.791002435033769657, -229.1824765006467715 ) ) ;
#12457 = DIRECTION ( 'NONE',  ( -1.000000000000000000, 0.000000000000000000, 0.000000000000000000 ) ) ;
#12458 = CARTESIAN_POINT ( 'NONE',  ( 16.91879448796214191, 0.8271603773820436212, -230.0510230802265710 ) ) ;
#12459 = EDGE_CURVE ( 'NONE', #16430, #21087, #16677, .T. ) ;
#12460 = CARTESIAN_POINT ( 'NONE',  ( 6.053458391837899910, -12.85229775019162268, -220.9645494416007523 ) ) ;
#12461 = FILL_AREA_STYLE ('',( #8970 ) ) ;
#12462 = CARTESIAN_POINT ( 'NONE',  ( -6.101488798441174310, 11.33371047077072369, -225.3616985956418546 ) ) ;
#12463 = PRODUCT_DEFINITION_FORMATION_WITH_SPECIFIED_SOURCE ( 'ANY', '', #10136, .NOT_KNOWN. ) ;
#12464 = CARTESIAN_POINT ( 'NONE',  ( -10.30034651166687887, 25.05454868506992838, -216.5587736482213188 ) ) ;
#12465 = ORIENTED_EDGE ( 'NONE', *, *, #18879, .T. ) ;
#12466 = CARTESIAN_POINT ( 'NONE',  ( -27.29953305526601426, 11.21644211419729054, -229.3676346105362995 ) ) ;
#12467 = CARTESIAN_POINT ( 'NONE',  ( -9.776740361816679936, -16.43846667899986258, -218.0739489017842061 ) ) ;
#12468 = CARTESIAN_POINT ( 'NONE',  ( -24.89698496326684207, -2.290081829390879342, -9.739783964571683939 ) ) ;
#12469 = CARTESIAN_POINT ( 'NONE',  ( 22.03647168421188596, 0.3315607655626346961, -232.0572713672587213 ) ) ;
#12470 = CARTESIAN_POINT ( 'NONE',  ( -15.20262116893801974, 8.038155052917188570, -217.6767387945475036 ) ) ;
#12471 = CARTESIAN_POINT ( 'NONE',  ( 4.894111852004805030, -16.26971588820515890, -218.1545738548100530 ) ) ;
#12472 =( NAMED_UNIT ( * ) PLANE_ANGLE_UNIT ( ) SI_UNIT ( $, .RADIAN. ) );
#12473 = CARTESIAN_POINT ( 'NONE',  ( 18.80464855560517989, -2.963306505625492804, -225.4831391053028824 ) ) ;
#12474 = CARTESIAN_POINT ( 'NONE',  ( 21.91535456744164279, 7.573568724377624406, -232.0371228855588868 ) ) ;
#12475 = CARTESIAN_POINT ( 'NONE',  ( -7.352050649209116884, 10.05454564170545417, -223.7370967983176229 ) ) ;
#12476 = CARTESIAN_POINT ( 'NONE',  ( 0.000000000000000000, 0.000000000000000000, -74.48236190979496030 ) ) ;
#12477 = CARTESIAN_POINT ( 'NONE',  ( 16.29563576379945999, 21.41235115595959826, -221.8114656550040991 ) ) ;
#12478 = CARTESIAN_POINT ( 'NONE',  ( -2.076897692258683925, -29.27639190819841275, -225.1343076284445601 ) ) ;
#12479 = ORIENTED_EDGE ( 'NONE', *, *, #2633, .T. ) ;
#12480 = CARTESIAN_POINT ( 'NONE',  ( 3.080453011304693511, 29.32691491905673331, -222.8956499783474499 ) ) ;
#12481 = CARTESIAN_POINT ( 'NONE',  ( -18.02718827071834085, 20.33515877052379395, -229.5060669840136143 ) ) ;
#12482 = CARTESIAN_POINT ( 'NONE',  ( -19.26845014167239611, 9.481468541508135672, -234.4856117705182328 ) ) ;
#12483 = CARTESIAN_POINT ( 'NONE',  ( -10.44804907229818980, -15.26164834479392240, -220.3887109030195859 ) ) ;
#12484 = CARTESIAN_POINT ( 'NONE',  ( -24.63401512838747820, 0.000000000000000000, 77.51594804401857175 ) ) ;
#12485 = EDGE_LOOP ( 'NONE', ( #22080, #14503, #11737, #3969 ) ) ;
#12486 = CARTESIAN_POINT ( 'NONE',  ( -18.71530386740073126, -0.6857509888707814527, -217.6195632122020527 ) ) ;
#12487 = CARTESIAN_POINT ( 'NONE',  ( 8.192339082998598698, -27.06056373437490947, -224.5174968915583236 ) ) ;
#12488 = CARTESIAN_POINT ( 'NONE',  ( 10.57926812561479757, 10.00910231482511215, -225.8341706491384286 ) ) ;
#12489 = CARTESIAN_POINT ( 'NONE',  ( -18.47334320050258327, 24.79293862780133040, -226.9986786077537317 ) ) ;
#12490 = CARTESIAN_POINT ( 'NONE',  ( 26.75877786246624623, 11.80320999550499117, -231.5572967531201414 ) ) ;
#12491 = CARTESIAN_POINT ( 'NONE',  ( 9.586902571418640662, 24.43292817174309661, -231.9968623198229807 ) ) ;
#12492 = CARTESIAN_POINT ( 'NONE',  ( 13.47875474198669821, 0.7946461602593113405, -222.1045510852317761 ) ) ;
#12493 = CARTESIAN_POINT ( 'NONE',  ( -8.803769170443210612, -17.82266517633203406, -233.6972128408098683 ) ) ;
#12494 = CARTESIAN_POINT ( 'NONE',  ( 19.68037530048075112, -17.97179847169212508, -231.8517058357153076 ) ) ;
#12495 = CARTESIAN_POINT ( 'NONE',  ( 0.000000000000000000, -21.99162546567091425, -78.50000000000000000 ) ) ;
#12496 = DIRECTION ( 'NONE',  ( -0.000000000000000000, -0.000000000000000000, -1.000000000000000000 ) ) ;
#12497 = CARTESIAN_POINT ( 'NONE',  ( -16.85225081326727903, 6.237400186851330020, -234.5847093771173206 ) ) ;
#12498 = CARTESIAN_POINT ( 'NONE',  ( -16.25683815890624473, -3.869351682469674980, -222.5551530127839044 ) ) ;
#12499 = CARTESIAN_POINT ( 'NONE',  ( -25.64868633208605786, 12.30364128039660798, -229.0020209687957049 ) ) ;
#12500 = CARTESIAN_POINT ( 'NONE',  ( 15.37089934297015503, 20.64239674606488961, -217.2018742121147170 ) ) ;
#12501 = CARTESIAN_POINT ( 'NONE',  ( 5.791579991237209235, 15.48299465423324861, -228.0203551130359472 ) ) ;
#12502 = EDGE_LOOP ( 'NONE', ( #14722, #1681, #2502, #12026 ) ) ;
#12503 = CARTESIAN_POINT ( 'NONE',  ( 8.679960083554519201, -14.04048791834972398, -217.5462328905347249 ) ) ;
#12504 = ORIENTED_EDGE ( 'NONE', *, *, #20966, .T. ) ;
#12505 = CARTESIAN_POINT ( 'NONE',  ( 15.87442104186276381, 8.674488492264579520, -230.9702037640878416 ) ) ;
#12506 = CARTESIAN_POINT ( 'NONE',  ( -19.90771709537278156, 23.83218599423810602, -225.0439263757368735 ) ) ;
#12507 = CARTESIAN_POINT ( 'NONE',  ( -17.94782256308196366, 19.07396065564992682, -232.7143578890335220 ) ) ;
#12508 = CARTESIAN_POINT ( 'NONE',  ( -25.34460520202507539, -7.988444519707189606, -217.6292756219348234 ) ) ;
#12509 = CARTESIAN_POINT ( 'NONE',  ( -26.74045434827795020, 12.41518252455047744, -220.4617428697642652 ) ) ;
#12510 = CARTESIAN_POINT ( 'NONE',  ( 15.96089671440110713, 1.143943728337336374, -218.3532651118343892 ) ) ;
#12511 = CARTESIAN_POINT ( 'NONE',  ( -10.65640919150578192, 23.79238421564942740, -218.1088542024188826 ) ) ;
#12512 = CARTESIAN_POINT ( 'NONE',  ( 24.61409543538958289, 19.88121288930873476, -228.5015986536257344 ) ) ;
#12513 = CARTESIAN_POINT ( 'NONE',  ( 19.29259174080182504, 0.5828707127177102931, -219.2781652733668807 ) ) ;
#12514 = CARTESIAN_POINT ( 'NONE',  ( -17.83852468596024110, -8.357198216422425219, -233.0481596892792879 ) ) ;
#12515 = CARTESIAN_POINT ( 'NONE',  ( 5.646952844456516019, 23.06006924884521325, -218.8221376988549878 ) ) ;
#12516 = CARTESIAN_POINT ( 'NONE',  ( -0.1947256686167265494, -30.94043057420685727, -223.1178397439027492 ) ) ;
#12517 = CARTESIAN_POINT ( 'NONE',  ( 4.343013938751969505, 13.02036404005131587, -224.7825435359082178 ) ) ;
#12518 = CARTESIAN_POINT ( 'NONE',  ( 15.81704710165450756, -18.55181613945514840, -214.8869746720286287 ) ) ;
#12519 = CARTESIAN_POINT ( 'NONE',  ( 22.00000000000000711, 0.000000000000000000, -233.0000000000000284 ) ) ;
#12520 = ADVANCED_FACE ( 'NONE', ( #16418 ), #21684, .T. ) ;
#12521 = CARTESIAN_POINT ( 'NONE',  ( -20.57288920227272655, 16.51351902378409520, -230.8484733908063333 ) ) ;
#12522 = DIRECTION ( 'NONE',  ( -0.000000000000000000, 0.000000000000000000, -1.000000000000000000 ) ) ;
#12523 = CARTESIAN_POINT ( 'NONE',  ( 19.75516891782859474, -3.344025276999063934, -216.3638920815759263 ) ) ;
#12524 = CARTESIAN_POINT ( 'NONE',  ( 2.445562843591592372, 25.89340784564244657, -229.2671352353737859 ) ) ;
#12525 = CARTESIAN_POINT ( 'NONE',  ( 19.55931020704464274, 3.833820734573247346, -215.4549349108404783 ) ) ;
#12527 = AXIS2_PLACEMENT_3D ( 'NONE', #15053, #11550, #16846 ) ;
#12526 = CARTESIAN_POINT ( 'NONE',  ( 17.00168025137501004, 6.212099629982537508, -219.0548246536471595 ) ) ;
#12528 = CARTESIAN_POINT ( 'NONE',  ( -15.95469971785872332, -24.72796590591627464, -225.3946449442874211 ) ) ;
#12529 = CARTESIAN_POINT ( 'NONE',  ( 9.400341091271927851, 28.64465517894215196, -231.0823126271420165 ) ) ;
#12530 = DIRECTION ( 'NONE',  ( 0.000000000000000000, 0.000000000000000000, 1.000000000000000000 ) ) ;
#12531 = CARTESIAN_POINT ( 'NONE',  ( 0.3555517721839966394, -12.99484957898737569, -222.7951259809431974 ) ) ;
#12532 = CARTESIAN_POINT ( 'NONE',  ( -14.22255565734842619, 21.32307452572284134, -218.8849463683180261 ) ) ;
#12533 = CARTESIAN_POINT ( 'NONE',  ( 16.10596270516584028, 24.75152718569329835, -228.9330127594856492 ) ) ;
#12534 = CARTESIAN_POINT ( 'NONE',  ( -21.99356461413155728, 5.827088221545293045, -219.1725956997024127 ) ) ;
#12535 = CIRCLE ( 'NONE', #3168, 14.50000000000000000 ) ;
#12536 = CARTESIAN_POINT ( 'NONE',  ( -10.83439284573031536, 18.36737820296253432, -234.3014274143859836 ) ) ;
#12537 = CARTESIAN_POINT ( 'NONE',  ( 20.88210880980788531, 0.9259446317980322139, -218.6312544800709929 ) ) ;
#12538 = CARTESIAN_POINT ( 'NONE',  ( 7.436546160899932367, -15.25288503996851475, -221.8354696069030467 ) ) ;
#12539 = ORIENTED_EDGE ( 'NONE', *, *, #1832, .T. ) ;
#12540 = CARTESIAN_POINT ( 'NONE',  ( 12.70013114424463296, -16.94540864491495924, -217.3462533088837745 ) ) ;
#12541 = CARTESIAN_POINT ( 'NONE',  ( 0.4762409465891800919, 16.20008108839776284, -225.9988706007428050 ) ) ;
#12542 = CARTESIAN_POINT ( 'NONE',  ( 26.00000000000000000, 1.360023205165816762E-13, 0.000000000000000000 ) ) ;
#12543 = CARTESIAN_POINT ( 'NONE',  ( 15.76910524310159900, 5.601482066865847820, -220.3440822020379528 ) ) ;
#12544 = CARTESIAN_POINT ( 'NONE',  ( -22.24434812881145618, 2.221346625544017961, -216.9231029185778254 ) ) ;
#12545 = CARTESIAN_POINT ( 'NONE',  ( -11.20272313682045073, -7.956653478762055087, -225.3025344850567819 ) ) ;
#12546 = CARTESIAN_POINT ( 'NONE',  ( 7.437838793555467731, -20.85539581353325289, -233.9154700400843865 ) ) ;
#12547 = CARTESIAN_POINT ( 'NONE',  ( -6.067446494494625142, 16.28408815813367028, -230.0786439517394513 ) ) ;
#12548 = CARTESIAN_POINT ( 'NONE',  ( 0.000000000000000000, 0.000000000000000000, 75.00000000000000000 ) ) ;
#12549 = CARTESIAN_POINT ( 'NONE',  ( 20.64430047260004031, 12.67811357335941480, -231.0449411089858813 ) ) ;
#12550 = CARTESIAN_POINT ( 'NONE',  ( -10.45786516112131892, 23.61456281964591852, -233.2869923610001592 ) ) ;
#12551 = CARTESIAN_POINT ( 'NONE',  ( -1.796846813493219619, 26.08418332695505271, -220.7262848173578504 ) ) ;
#12552 = ORIENTED_EDGE ( 'NONE', *, *, #19039, .T. ) ;
#12553 = CARTESIAN_POINT ( 'NONE',  ( 2.485733319737138736, 14.76073968410796056, -221.5245536174130905 ) ) ;
#12554 = CARTESIAN_POINT ( 'NONE',  ( 17.57135037026572277, 0.09191994211922807634, -232.8447871904542410 ) ) ;
#12555 = CARTESIAN_POINT ( 'NONE',  ( 17.96045420455031305, -0.3746358454349600908, -217.9627609769914613 ) ) ;
#12556 = CARTESIAN_POINT ( 'NONE',  ( 17.47229821656412341, -21.26691171910925249, -219.4940788861217413 ) ) ;
#12557 = DIRECTION ( 'NONE',  ( 0.1736481776669307198, 0.000000000000000000, 0.9848077530122080203 ) ) ;
#12558 = DIRECTION ( 'NONE',  ( -1.000000000000000000, 0.000000000000000000, 0.000000000000000000 ) ) ;
#12559 = EDGE_CURVE ( 'NONE', #15541, #5788, #5161, .T. ) ;
#12560 = CARTESIAN_POINT ( 'NONE',  ( 5.248230734842167955, 23.54336384919183445, -216.8914391693808739 ) ) ;
#12561 = CARTESIAN_POINT ( 'NONE',  ( 19.53765964318905546, -5.556987368099968627, -230.7409885362571345 ) ) ;
#12562 = DIRECTION ( 'NONE',  ( 1.000000000000000000, -0.000000000000000000, -0.000000000000000000 ) ) ;
#12563 = CARTESIAN_POINT ( 'NONE',  ( 15.10937218716165020, -26.44221868192832758, -222.7999243300199907 ) ) ;
#12564 =( NAMED_UNIT ( * ) PLANE_ANGLE_UNIT ( ) SI_UNIT ( $, .RADIAN. ) );
#12565 = CARTESIAN_POINT ( 'NONE',  ( -10.45786516112131892, 23.61456281964591852, -233.2869923610001592 ) ) ;
#12566 = CARTESIAN_POINT ( 'NONE',  ( -8.123851230256436295, 20.56863949923577550, -215.0796075421103239 ) ) ;
#12567 = ORIENTED_EDGE ( 'NONE', *, *, #21369, .T. ) ;
#12568 = CARTESIAN_POINT ( 'NONE',  ( -13.58874046263339608, 12.73011668665171392, -216.5659449791897941 ) ) ;
#12569 = CARTESIAN_POINT ( 'NONE',  ( -11.57846532275044460, -10.37575015818511304, -229.3776965522603462 ) ) ;
#12570 = LINE ( 'NONE', #17969, #15231 ) ;
#12571 = ADVANCED_FACE ( 'NONE', ( #1328 ), #6615, .F. ) ;
#12572 = CARTESIAN_POINT ( 'NONE',  ( -22.38029933203972277, 5.310221276841376792, -8.479724577993932755 ) ) ;
#12573 = CARTESIAN_POINT ( 'NONE',  ( -18.08305592660031991, 4.022743421239192152, -217.2335041149100050 ) ) ;
#12574 = CARTESIAN_POINT ( 'NONE',  ( 8.479858146824877707, -14.20649975585062563, -220.0175458633526091 ) ) ;
#12575 = SURFACE_STYLE_FILL_AREA ( #10879 ) ;
#12576 = CARTESIAN_POINT ( 'NONE',  ( -11.67631226053870996, 6.737291529340801333, -227.3110382950315227 ) ) ;
#12577 = CARTESIAN_POINT ( 'NONE',  ( 19.79854089336508594, 4.557290221971136646, -217.3342919181881143 ) ) ;
#12578 = CARTESIAN_POINT ( 'NONE',  ( -22.56222084847001597, 18.89892770556097901, -231.8972396388394088 ) ) ;
#12579 = FACE_BOUND ( 'NONE', #15188, .T. ) ;
#12580 = CARTESIAN_POINT ( 'NONE',  ( 10.79895562092076844, 12.01490073542734116, -225.7380208924852809 ) ) ;
#12581 = CARTESIAN_POINT ( 'NONE',  ( -0.6720842648862578317, -17.90033647106004011, -231.4757128331908973 ) ) ;
#12582 = ORIENTED_EDGE ( 'NONE', *, *, #10591, .F. ) ;
#12583 = CARTESIAN_POINT ( 'NONE',  ( 2.951582164238582440, 19.39026647431845873, -217.4356918981242472 ) ) ;
#12584 = CARTESIAN_POINT ( 'NONE',  ( -9.969679877803788060, 12.84542071557917176, -220.4758784541224657 ) ) ;
#12585 = CARTESIAN_POINT ( 'NONE',  ( -10.94147694953847250, 13.90730769817462864, -218.7797619932150042 ) ) ;
#12586 = CARTESIAN_POINT ( 'NONE',  ( -13.63268120803286720, -13.08481847960132249, -219.9337478264210404 ) ) ;
#12587 = DIRECTION ( 'NONE',  ( -0.000000000000000000, -0.000000000000000000, -1.000000000000000000 ) ) ;
#12588 = EDGE_LOOP ( 'NONE', ( #7279, #9346 ) ) ;
#12589 = CARTESIAN_POINT ( 'NONE',  ( -13.93333636822611155, 3.327141996558931947, -221.4468162587888287 ) ) ;
#12590 = CARTESIAN_POINT ( 'NONE',  ( 7.754512012237808172, -26.66010948812077430, -222.3649102068104924 ) ) ;
#12591 = CARTESIAN_POINT ( 'NONE',  ( 26.48990917286906921, 12.16675355942207659, -225.0153622588060216 ) ) ;
#12592 = CARTESIAN_POINT ( 'NONE',  ( -3.082945806077231676, 30.69897765966285874, -224.2387254578930822 ) ) ;
#12593 = UNCERTAINTY_MEASURE_WITH_UNIT (LENGTH_MEASURE( 1.000000000000000082E-05 ), #18657, 'distance_accuracy_value', 'NONE');
#12594 = CARTESIAN_POINT ( 'NONE',  ( -27.32994399549947673, 3.379920396491164603, -227.9326384921875217 ) ) ;
#12595 = EDGE_CURVE ( 'NONE', #16686, #3236, #15614, .T. ) ;
#12596 = CARTESIAN_POINT ( 'NONE',  ( 5.017623471397871349, 29.83561274492976878, -222.9769172135417250 ) ) ;
#12597 = CARTESIAN_POINT ( 'NONE',  ( 13.51280905378919606, 1.666897247961874884, -222.5030422686260465 ) ) ;
#12598 = CARTESIAN_POINT ( 'NONE',  ( -17.42499862437977853, -18.98713029041037004, -232.7811807006768845 ) ) ;
#12599 = CARTESIAN_POINT ( 'NONE',  ( 15.84759643368428428, -7.142586963752317608, -231.1761396821659673 ) ) ;
#12600 =( REPRESENTATION_RELATIONSHIP ('NONE','NONE', #5277, #9901 ) REPRESENTATION_RELATIONSHIP_WITH_TRANSFORMATION ( #21871 )SHAPE_REPRESENTATION_RELATIONSHIP( ) );
#12601 = FACE_BOUND ( 'NONE', #19172, .T. ) ;
#12602 = LINE ( 'NONE', #21030, #5828 ) ;
#12603 = CARTESIAN_POINT ( 'NONE',  ( -21.64120863631820413, 17.87363223393748868, -233.1390268986752119 ) ) ;
#12604 = CARTESIAN_POINT ( 'NONE',  ( -16.74998343472315199, -3.152285961911668988, -228.0274629056708022 ) ) ;
#12605 = CARTESIAN_POINT ( 'NONE',  ( -20.57288920227272655, 16.51351902378409520, -230.8484733908063333 ) ) ;
#12606 = CARTESIAN_POINT ( 'NONE',  ( 27.79746884017060538, 13.63637251724950339, -226.5788410723774575 ) ) ;
#12607 = CARTESIAN_POINT ( 'NONE',  ( 0.3355639943343493026, 23.87279439325363128, -218.0067922387550823 ) ) ;
#12608 = ORIENTED_EDGE ( 'NONE', *, *, #16711, .F. ) ;
#12609 = CARTESIAN_POINT ( 'NONE',  ( 10.18197402670511842, -10.22146582328408115, -231.5691222609812598 ) ) ;
#12610 = CARTESIAN_POINT ( 'NONE',  ( 28.51464931495100785, 5.422321182929326966, -223.8116416110474347 ) ) ;
#12611 = CARTESIAN_POINT ( 'NONE',  ( -0.04850409037381671340, 14.20520396026658716, -231.8092226852533031 ) ) ;
#12612 = CARTESIAN_POINT ( 'NONE',  ( -3.309130212696198559, 28.80211350556483296, -217.4284252357080334 ) ) ;
#12613 = CARTESIAN_POINT ( 'NONE',  ( -11.96453848309674228, -6.796862595549911568, -223.8262896469332759 ) ) ;
#12614 = CARTESIAN_POINT ( 'NONE',  ( -13.83274569775339202, 16.20364235096346661, -234.0851861771356539 ) ) ;
#12615 = CARTESIAN_POINT ( 'NONE',  ( -6.453512288987201195, -13.27786176931083340, 93.00000000000000000 ) ) ;
#12616 = CONICAL_SURFACE ( 'NONE', #2888, 23.03038449397558196, 0.1745329251994333364 ) ;
#12617 = CARTESIAN_POINT ( 'NONE',  ( 24.56541673123750158, -5.996287403333383281, -231.6940117905984664 ) ) ;
#12618 = CARTESIAN_POINT ( 'NONE',  ( 1.867752180833619713, 31.25122076096762669, -227.4007918511463231 ) ) ;
#12619 = CARTESIAN_POINT ( 'NONE',  ( 26.50744623559791435, 1.694095366541529923, -217.6968951254705473 ) ) ;
#12620 = CARTESIAN_POINT ( 'NONE',  ( 28.56567312134318826, 3.451746495494312672, -224.1550573921799412 ) ) ;
#12621 = CARTESIAN_POINT ( 'NONE',  ( 12.58590500897257947, 11.38573988265384607, -230.4867078522624695 ) ) ;
#12622 = CARTESIAN_POINT ( 'NONE',  ( -17.60306105620566441, -10.62493847279374926, -216.8163279515337649 ) ) ;
#12623 = ORIENTED_EDGE ( 'NONE', *, *, #20925, .T. ) ;
#12624 = CARTESIAN_POINT ( 'NONE',  ( 4.936777854427027989, 27.97379167488809060, -227.0886654730259124 ) ) ;
#12625 = CARTESIAN_POINT ( 'NONE',  ( -1.542335193334551491, -19.71915426430242135, -216.1352730594569209 ) ) ;
#12626 = CARTESIAN_POINT ( 'NONE',  ( 14.39473142419577023, 15.98257177912839389, -217.4557725731239373 ) ) ;
#12627 = CARTESIAN_POINT ( 'NONE',  ( 7.141633727147962851, -29.98958059360777639, -229.8804610602846594 ) ) ;
#12628 = FACE_OUTER_BOUND ( 'NONE', #11177, .T. ) ;
#12629 = CARTESIAN_POINT ( 'NONE',  ( -12.87285471141929172, 9.485162256560764504, -229.1865421006261840 ) ) ;
#12630 =( NAMED_UNIT ( * ) SI_UNIT ( $, .STERADIAN. ) SOLID_ANGLE_UNIT ( ) );
#12631 = CARTESIAN_POINT ( 'NONE',  ( -22.94312929380076937, -2.351969141711130806, -217.0768970835230505 ) ) ;
#12632 = CARTESIAN_POINT ( 'NONE',  ( 12.83388873239664996, 22.07510045760132655, -230.4740059944613222 ) ) ;
#12633 = CARTESIAN_POINT ( 'NONE',  ( -12.05423124486310904, 12.38527783110887803, -219.7419643105747014 ) ) ;
#12634 = CARTESIAN_POINT ( 'NONE',  ( -17.92628912275201003, -0.6090139417824500523, -215.7724435048976943 ) ) ;
#12635 = CARTESIAN_POINT ( 'NONE',  ( -8.288471666609035893, -17.31860360376325403, -217.6655967056599366 ) ) ;
#12636 = CARTESIAN_POINT ( 'NONE',  ( 27.79290571682592770, 12.05347838982552666, -230.1298045326732051 ) ) ;
#12637 = DIRECTION ( 'NONE',  ( 0.000000000000000000, 0.000000000000000000, -1.000000000000000000 ) ) ;
#12638 = CARTESIAN_POINT ( 'NONE',  ( -10.91546170668013005, -7.896971223757457636, -230.5866998909293102 ) ) ;
#12639 = CARTESIAN_POINT ( 'NONE',  ( 7.772443558932104146, 25.24620711463332157, -231.7813173736589931 ) ) ;
#12640 = CARTESIAN_POINT ( 'NONE',  ( 11.43247012502872728, 12.44034019618676190, -231.9336559008378629 ) ) ;
#12641 = VECTOR ( 'NONE', #20198, 1000.000000000000227 ) ;
#12642 = CARTESIAN_POINT ( 'NONE',  ( -15.15469129103955304, 15.56563882170958024, -231.6314069158229643 ) ) ;
#12643 = EDGE_CURVE ( 'NONE', #8526, #21835, #6842, .T. ) ;
#12644 = CARTESIAN_POINT ( 'NONE',  ( 3.044038000507106378, 30.22621415828681180, -231.1553244844465382 ) ) ;
#12645 = CARTESIAN_POINT ( 'NONE',  ( 15.18181359483165949, 6.369295616116027681, -230.7949408486033462 ) ) ;
#12646 = VERTEX_POINT ( 'NONE', #4805 ) ;
#12647 = CARTESIAN_POINT ( 'NONE',  ( 15.70595326690115634, -18.65841243762358559, -219.6423885132037981 ) ) ;
#12648 = CARTESIAN_POINT ( 'NONE',  ( 5.452943511046377090, -14.64908918772281865, -221.6090591728701611 ) ) ;
#12649 = CARTESIAN_POINT ( 'NONE',  ( -20.99999999999999645, 0.000000000000000000, 69.99999999999998579 ) ) ;
#12650 = CIRCLE ( 'NONE', #12283, 3.000000000000002665 ) ;
#12651 = CARTESIAN_POINT ( 'NONE',  ( 21.31262902390056624, 0.4111834581965390645, -232.0572713672585792 ) ) ;
#12652 = CARTESIAN_POINT ( 'NONE',  ( 14.62702828724412285, -1.994068170757606673, -224.0552340365271959 ) ) ;
#12653 = CARTESIAN_POINT ( 'NONE',  ( -12.13177435108894642, -8.392035797555511323, -228.8392847287196332 ) ) ;
#12654 = CARTESIAN_POINT ( 'NONE',  ( 1.292981098121811279, -26.53499626907933262, -232.9055005154886828 ) ) ;
#12655 = CARTESIAN_POINT ( 'NONE',  ( 6.295505112925526170, 15.36201163567862693, -221.5772643759389098 ) ) ;
#12656 = CARTESIAN_POINT ( 'NONE',  ( 0.000000000000000000, 0.000000000000000000, -55.00000000000000000 ) ) ;
#12657 = CARTESIAN_POINT ( 'NONE',  ( -11.30246491834384770, 5.534029070539333794, -225.8243940897388597 ) ) ;
#12658 = CARTESIAN_POINT ( 'NONE',  ( -7.825349071214003693, 24.14595706726266755, -216.5959661901539732 ) ) ;
#12659 = CARTESIAN_POINT ( 'NONE',  ( 0.4762409465891800919, 16.20008108839776284, -225.9988706007428050 ) ) ;
#12660 = CARTESIAN_POINT ( 'NONE',  ( -24.25245498015852874, 0.2109992039763788352, -218.1398602137601301 ) ) ;
#12661 = ORIENTED_EDGE ( 'NONE', *, *, #11585, .T. ) ;
#12662 = CARTESIAN_POINT ( 'NONE',  ( 14.60728983664449387, 19.38727400458104455, -216.6381802409380555 ) ) ;
#12663 = CARTESIAN_POINT ( 'NONE',  ( -15.82068653568960137, 8.372322471091806051, -220.7139663195713979 ) ) ;
#12664 = CARTESIAN_POINT ( 'NONE',  ( 12.66989206167516357, 2.082990619159506007, -225.6419847029432901 ) ) ;
#12665 = CARTESIAN_POINT ( 'NONE',  ( 2.283233934795953601, -16.37150177406293849, -220.5471140349473842 ) ) ;
#12666 = DIRECTION ( 'NONE',  ( 0.000000000000000000, 0.000000000000000000, 1.000000000000000000 ) ) ;
#12667 = VERTEX_POINT ( 'NONE', #15178 ) ;
#12668 = TOROIDAL_SURFACE ( 'NONE', #16994, 13.12488928717151637, 5.000000000000000000 ) ;
#12669 = CARTESIAN_POINT ( 'NONE',  ( 13.43170911749896490, 19.07691563292472026, -232.7497845103644636 ) ) ;
#12670 = CARTESIAN_POINT ( 'NONE',  ( -17.01570095888788003, -2.024181990473361115, -234.1256067144893791 ) ) ;
#12671 = CARTESIAN_POINT ( 'NONE',  ( -15.30864812529618391, 1.596444765892653717, -220.3859421844601627 ) ) ;
#12672 = CARTESIAN_POINT ( 'NONE',  ( -1.177898122437396333, -26.14463525305933445, -216.8677949074964033 ) ) ;
#12673 = PRODUCT_CONTEXT ( 'NONE', #4528, 'mechanical' ) ;
#12674 = CARTESIAN_POINT ( 'NONE',  ( -11.26857159993117996, 28.96895336474501192, -225.6039696848669678 ) ) ;
#12675 = CARTESIAN_POINT ( 'NONE',  ( -21.66801938871533650, 16.28801167444048659, -218.5240035253498547 ) ) ;
#12676 = ORIENTED_EDGE ( 'NONE', *, *, #1423, .T. ) ;
#12677 = CARTESIAN_POINT ( 'NONE',  ( -15.48255455842386219, 10.01793346089237069, -233.1197357361336913 ) ) ;
#12678 = CARTESIAN_POINT ( 'NONE',  ( -10.06927776881013514, -17.00317020600589402, -217.8513858272130790 ) ) ;
#12679 = DIRECTION ( 'NONE',  ( -1.000000000000000000, 0.000000000000000000, 0.000000000000000000 ) ) ;
#12680 = CARTESIAN_POINT ( 'NONE',  ( -22.77746302204332451, 3.250740792401631829, -9.479807400168150266 ) ) ;
#12681 = CARTESIAN_POINT ( 'NONE',  ( -10.30050448363967419, 10.07750059423401190, -220.1837019037183723 ) ) ;
#12682 = CARTESIAN_POINT ( 'NONE',  ( 7.813662449283098610, -13.08401493520405445, -221.9442578939891177 ) ) ;
#12683 = EDGE_CURVE ( 'NONE', #12453, #15721, #19595, .T. ) ;
#12684 = CARTESIAN_POINT ( 'NONE',  ( -19.25929423112888017, 9.818144317380269825, -216.1837936240308409 ) ) ;
#12685 = TOROIDAL_SURFACE ( 'NONE', #19127, 24.63401512838748530, 3.000000000000004441 ) ;
#12686 = CARTESIAN_POINT ( 'NONE',  ( -13.63442241228529994, 1.608023091903783008, -219.2326980015357094 ) ) ;
#12687 = CARTESIAN_POINT ( 'NONE',  ( -1.336753021691559962, 16.04398320409420720, -230.2310715620304507 ) ) ;
#12688 = FACE_OUTER_BOUND ( 'NONE', #20377, .T. ) ;
#12689 = CARTESIAN_POINT ( 'NONE',  ( 14.65309016725241698, 3.424799466898550637, -221.5217808432381048 ) ) ;
#12690 = CARTESIAN_POINT ( 'NONE',  ( -14.13544422886439911, -23.73189729233824252, -223.0800202563271171 ) ) ;
#12691 = ORIENTED_EDGE ( 'NONE', *, *, #16077, .T. ) ;
#12692 = CARTESIAN_POINT ( 'NONE',  ( -6.720912670637915198, 19.69156892798266512, -217.8848069150180891 ) ) ;
#12693 = CARTESIAN_POINT ( 'NONE',  ( -10.07004052286948337, 22.64471483900350179, -217.4645417110143626 ) ) ;
#12694 = CARTESIAN_POINT ( 'NONE',  ( -10.52776196018457711, 13.57482816453351937, -219.2327734183297423 ) ) ;
#12695 = VERTEX_POINT ( 'NONE', #20438 ) ;
#12696 = CARTESIAN_POINT ( 'NONE',  ( -9.770823421170108602, -12.84821564276127503, -225.3905567659999178 ) ) ;
#12697 = CYLINDRICAL_SURFACE ( 'NONE', #21868, 10.00000000000000000 ) ;
#12698 = ORIENTED_EDGE ( 'NONE', *, *, #4652, .F. ) ;
#12699 = CARTESIAN_POINT ( 'NONE',  ( -14.87984907657228639, 0.2138881189739126887, -228.7773920408832282 ) ) ;
#12700 = CARTESIAN_POINT ( 'NONE',  ( -1.243024450407066439, -19.42038079238686876, -231.9048276842376595 ) ) ;
#12701 = CARTESIAN_POINT ( 'NONE',  ( 18.29617186523616468, 23.20920553663278341, -223.4372550713720216 ) ) ;
#12702 = CARTESIAN_POINT ( 'NONE',  ( 0.9908753270255351575, 13.79205759140780430, -228.0165926715089881 ) ) ;
#12703 = CIRCLE ( 'NONE', #1567, 21.80000000000008598 ) ;
#12704 = AXIS2_PLACEMENT_3D ( 'NONE', #7873, #4357, #6280 ) ;
#12705 = CARTESIAN_POINT ( 'NONE',  ( -23.30382222616342247, 9.914163031146200566, -218.5285240371296425 ) ) ;
#12706 = CARTESIAN_POINT ( 'NONE',  ( 21.14441169763230732, 12.98245189690719315, -217.0976687089155064 ) ) ;
#12707 = CARTESIAN_POINT ( 'NONE',  ( 18.76922974182421555, 13.12635134380198210, -217.8010375391909008 ) ) ;
#12708 = DIRECTION ( 'NONE',  ( -1.224646799147353207E-16, 1.000000000000000000, 3.540705920434612608E-33 ) ) ;
#12709 = CARTESIAN_POINT ( 'NONE',  ( -13.05629324012484282, -10.24599397043673221, -218.7452066004821347 ) ) ;
#12710 = CARTESIAN_POINT ( 'NONE',  ( 1.623338700557370951, -21.82196275546919040, -234.1129525514646730 ) ) ;
#12711 = FACE_OUTER_BOUND ( 'NONE', #17568, .T. ) ;
#12712 = DIRECTION ( 'NONE',  ( -0.000000000000000000, 0.000000000000000000, -1.000000000000000000 ) ) ;
#12713 = CARTESIAN_POINT ( 'NONE',  ( -7.099035520468861549, 19.73710792467281649, -233.8745459908100770 ) ) ;
#12714 = CARTESIAN_POINT ( 'NONE',  ( 13.85225051576513700, -1.547701942753643145, -218.6451083988944788 ) ) ;
#12715 = CIRCLE ( 'NONE', #21677, 3.000000000000002665 ) ;
#12716 = TOROIDAL_SURFACE ( 'NONE', #17025, 24.63401512838761320, 3.000000000000035083 ) ;
#12717 = CARTESIAN_POINT ( 'NONE',  ( 10.95881707662767290, 12.06788758096456782, -231.4359029166177208 ) ) ;
#12718 = CARTESIAN_POINT ( 'NONE',  ( 10.32480721127626033, 15.84468581819879773, -230.0799086455579072 ) ) ;
#12719 = VERTEX_POINT ( 'NONE', #20210 ) ;
#12720 = CARTESIAN_POINT ( 'NONE',  ( 11.84677440217253341, -6.023754617643652054, -230.4469913264703962 ) ) ;
#12721 = CARTESIAN_POINT ( 'NONE',  ( 16.00819137755116373, 4.595691552992191120, -229.5669508871464757 ) ) ;
#12722 = CARTESIAN_POINT ( 'NONE',  ( -1.584125552723561592, 20.48724127025963782, -214.7515060525244621 ) ) ;
#12723 = CARTESIAN_POINT ( 'NONE',  ( -11.59874896804548250, 27.28969409813203484, -218.8626241359735332 ) ) ;
#12724 = CARTESIAN_POINT ( 'NONE',  ( -24.65069530437947876, -0.7989515219415058711, -216.4419420286324112 ) ) ;
#12725 = EDGE_CURVE ( 'NONE', #2304, #1564, #5027, .T. ) ;
#12726 = CARTESIAN_POINT ( 'NONE',  ( -17.65835845419170624, 22.55329142274348442, -231.2673511165784532 ) ) ;
#12727 = DIRECTION ( 'NONE',  ( -0.2588190451025213501, 0.000000000000000000, 0.9659258262890680902 ) ) ;
#12728 = EDGE_CURVE ( 'NONE', #21223, #13423, #12013, .T. ) ;
#12729 = CARTESIAN_POINT ( 'NONE',  ( 25.69761320619099720, -8.403105518750903613, -219.2599777650661110 ) ) ;
#12730 = EDGE_CURVE ( 'NONE', #351, #324, #7706, .T. ) ;
#12731 = CARTESIAN_POINT ( 'NONE',  ( -1.585416880194127520, 15.28258783379090424, -231.0852564988603319 ) ) ;
#12732 = CARTESIAN_POINT ( 'NONE',  ( 27.08260752785270853, 4.114838227474355570, -232.2882281786467331 ) ) ;
#12733 = CARTESIAN_POINT ( 'NONE',  ( -22.04257564474043818, 18.72061943465525857, -219.1781831295219263 ) ) ;
#12734 = VECTOR ( 'NONE', #8870, 1000.000000000000000 ) ;
#12735 = CARTESIAN_POINT ( 'NONE',  ( 11.33210854356620523, 22.81476816607802149, -217.8536224460118262 ) ) ;
#12736 = LINE ( 'NONE', #11378, #6935 ) ;
#12737 = CARTESIAN_POINT ( 'NONE',  ( -1.336753021691559962, 16.04398320409420720, -230.2310715620304507 ) ) ;
#12738 = CARTESIAN_POINT ( 'NONE',  ( -14.40111287326894640, -6.123720356435734757, -220.5571602876142094 ) ) ;
#12739 = CARTESIAN_POINT ( 'NONE',  ( 3.763426558366607111, 28.60172112197566818, -230.1816715025297526 ) ) ;
#12740 = CARTESIAN_POINT ( 'NONE',  ( 9.191046577198441980, -13.34937224525895161, -233.4761082295262611 ) ) ;
#12741 = CARTESIAN_POINT ( 'NONE',  ( 22.00000000000000000, 0.000000000000000000, -221.9999999999999716 ) ) ;
#12742 = CARTESIAN_POINT ( 'NONE',  ( -21.23733589435050817, 17.25275849955597351, -229.9547908233139708 ) ) ;
#12743 = CARTESIAN_POINT ( 'NONE',  ( 12.90474009670415967, -3.145873754258878385, -224.5449843457338375 ) ) ;
#12744 = CARTESIAN_POINT ( 'NONE',  ( 6.729623925010410623, 16.84721552001897038, -219.9221131804260381 ) ) ;
#12745 = CARTESIAN_POINT ( 'NONE',  ( -22.07068341299880743, 18.38202870573248049, -227.7785760498121306 ) ) ;
#12746 = CARTESIAN_POINT ( 'NONE',  ( -11.80036766549451599, 3.629178540272184783, -221.4826559383200220 ) ) ;
#12747 = CARTESIAN_POINT ( 'NONE',  ( -8.537495277687638051, -14.12518193842558212, -230.5589415009361858 ) ) ;
#12748 = CARTESIAN_POINT ( 'NONE',  ( 10.90540179105271967, 5.382827416078996841, -224.1493061458977820 ) ) ;
#12749 = COLOUR_RGB ( '', 0.40784314, 0.44705882, 0.49803922) ;
#12750 = CARTESIAN_POINT ( 'NONE',  ( 2.100000000000000089, 0.000000000000000000, -126.0000000000000284 ) ) ;
#12751 = CARTESIAN_POINT ( 'NONE',  ( -20.52308621596579030, -13.62600152083235905, -234.9101091540371442 ) ) ;
#12752 = CARTESIAN_POINT ( 'NONE',  ( -0.1881941282075867139, 17.37563936270229092, -230.9177995227891813 ) ) ;
#12753 = CARTESIAN_POINT ( 'NONE',  ( 13.16746181015946959, 0.3897807143096829741, -227.1676274388083243 ) ) ;
#12754 = CARTESIAN_POINT ( 'NONE',  ( -6.255852670334142829, 13.96671599789818252, -220.4426911866496823 ) ) ;
#12755 = CARTESIAN_POINT ( 'NONE',  ( 13.09827881591457022, 28.40264942367575784, -221.1045935444571455 ) ) ;
#12756 = CARTESIAN_POINT ( 'NONE',  ( 19.30248206944178335, -1.297331563427565726, -230.8957665284791290 ) ) ;
#12757 = CARTESIAN_POINT ( 'NONE',  ( -3.917974041549708630, -18.23196399112299559, -217.4080104222929606 ) ) ;
#12758 = CARTESIAN_POINT ( 'NONE',  ( 2.936803900436826709, -18.74190719154852758, -218.5197582523356061 ) ) ;
#12759 = CARTESIAN_POINT ( 'NONE',  ( 0.000000000000000000, 0.000000000000000000, -77.51594804401857175 ) ) ;
#12760 = CARTESIAN_POINT ( 'NONE',  ( 24.58316096239279602, 5.861425670879941485, -231.3104446318280623 ) ) ;
#12761 = CARTESIAN_POINT ( 'NONE',  ( 11.31395536621571019, -8.070181239749643964, -225.0898076798974614 ) ) ;
#12762 = CARTESIAN_POINT ( 'NONE',  ( -11.07688804854283049, -12.81333559660784971, -232.1241261852632363 ) ) ;
#12763 = AXIS2_PLACEMENT_3D ( 'NONE', #18000, #12929, #19775 ) ;
#12764 = CARTESIAN_POINT ( 'NONE',  ( -6.052919920376759855, -15.38051382379660836, -218.0337201863237624 ) ) ;
#12765 =( GEOMETRIC_REPRESENTATION_CONTEXT ( 3 ) GLOBAL_UNCERTAINTY_ASSIGNED_CONTEXT ( ( #17775 ) ) GLOBAL_UNIT_ASSIGNED_CONTEXT ( ( #3556, #12564, #3993 ) ) REPRESENTATION_CONTEXT ( 'NONE', 'WORKASPACE' ) );
#12766 = CARTESIAN_POINT ( 'NONE',  ( 3.325336547283623378, 18.92213121405483633, -219.7480163085221818 ) ) ;
#12767 = CARTESIAN_POINT ( 'NONE',  ( 0.000000000000000000, 0.000000000000000000, -75.00000000000000000 ) ) ;
#12768 = CARTESIAN_POINT ( 'NONE',  ( -16.36835685385702988, 8.002698209344293545, -233.7585018083067894 ) ) ;
#12769 = CARTESIAN_POINT ( 'NONE',  ( -5.807479211365208727, 19.77444019604324410, -216.0778658752277863 ) ) ;
#12770 = CARTESIAN_POINT ( 'NONE',  ( -2.015708574708954259, 26.78900769828807782, -221.5371848586876808 ) ) ;
#12771 = CARTESIAN_POINT ( 'NONE',  ( 27.20328812258980378, -0.4806365347271125965, -218.3128023695579998 ) ) ;
#12772 = ORIENTED_EDGE ( 'NONE', *, *, #6914, .T. ) ;
#12773 = CARTESIAN_POINT ( 'NONE',  ( 14.20064147608437821, 14.63411858269657806, -233.6150408276221242 ) ) ;
#12774 = CARTESIAN_POINT ( 'NONE',  ( -15.50322565568834321, 9.749075856218723857, -229.6019304695566916 ) ) ;
#12775 = CARTESIAN_POINT ( 'NONE',  ( 13.12946830070648652, 6.370976456471619365, -231.5124810213676483 ) ) ;
#12776 = CARTESIAN_POINT ( 'NONE',  ( 1.102456202203287550, -23.13885590315818064, -232.0370787247644557 ) ) ;
#12777 = DIRECTION ( 'NONE',  ( 6.123233995736766036E-17, -0.000000000000000000, -1.000000000000000000 ) ) ;
#12778 = DIRECTION ( 'NONE',  ( -0.9940043559354330149, -0.1093404791528966163, -6.737719923507020479E-14 ) ) ;
#12779 = CARTESIAN_POINT ( 'NONE',  ( 18.23324537670537993, 23.47692953258263771, -224.8333321331434433 ) ) ;
#12780 = CARTESIAN_POINT ( 'NONE',  ( 20.53618124091710939, -19.36892006637360097, -226.5121684596580849 ) ) ;
#12781 = FACE_OUTER_BOUND ( 'NONE', #20760, .T. ) ;
#12782 = AXIS2_PLACEMENT_3D ( 'NONE', #18875, #20999, #6955 ) ;
#12783 = AXIS2_PLACEMENT_3D ( 'NONE', #18612, #13659, #17037 ) ;
#12784 = CARTESIAN_POINT ( 'NONE',  ( -15.48425879135615446, -25.29886615046042309, -220.6886037686364261 ) ) ;
#12785 = ITEM_DEFINED_TRANSFORMATION ( 'NONE', 'NONE', #13854,  #6677 ) ;
#12786 = CARTESIAN_POINT ( 'NONE',  ( 4.484811161826725900, 15.38298568785217313, -219.4617573400562662 ) ) ;
#12787 = CARTESIAN_POINT ( 'NONE',  ( -4.334570222994868161, 11.62786715207288601, -222.6396919303362267 ) ) ;
#12788 = ORIENTED_EDGE ( 'NONE', *, *, #6538, .T. ) ;
#12789 = CARTESIAN_POINT ( 'NONE',  ( -6.855867220396999251, 12.17758473459128332, -220.6375607554995213 ) ) ;
#12790 = CARTESIAN_POINT ( 'NONE',  ( 28.44445586451508845, -4.662230540760189612, -220.9797193573593290 ) ) ;
#12791 = DIRECTION ( 'NONE',  ( -1.000000000000000000, 0.000000000000000000, -0.000000000000000000 ) ) ;
#12792 = CARTESIAN_POINT ( 'NONE',  ( -20.95684706105100759, 9.480813542266940175, -3.246593753853921349 ) ) ;
#12793 = CARTESIAN_POINT ( 'NONE',  ( -2.698926868850080041, 12.89339462271858316, -226.7595176699009585 ) ) ;
#12794 = CARTESIAN_POINT ( 'NONE',  ( 7.829076659910394476, -15.59360078984655651, -230.7142312655459762 ) ) ;
#12795 = SURFACE_STYLE_USAGE ( .BOTH. , #2101 ) ;
#12796 = CARTESIAN_POINT ( 'NONE',  ( -19.00318367631585659, 13.14621133775862916, -233.8403879275295765 ) ) ;
#12797 = CARTESIAN_POINT ( 'NONE',  ( -21.39667546302236900, 3.687493526428279100, -235.1435990565495047 ) ) ;
#12798 = CARTESIAN_POINT ( 'NONE',  ( -6.702936938788568888, 25.88675107068059944, -218.1129661040884287 ) ) ;
#12799 = CARTESIAN_POINT ( 'NONE',  ( -2.000000000000000000, 2.449293598294706414E-16, -120.0000000000000142 ) ) ;
#12800 = CARTESIAN_POINT ( 'NONE',  ( 28.52435124311170966, 7.611291969169514005, -224.8315247833735384 ) ) ;
#12801 = CARTESIAN_POINT ( 'NONE',  ( -7.205518813659622879, -14.37210213534873482, -226.5338589405291998 ) ) ;
#12802 = MECHANICAL_DESIGN_GEOMETRIC_PRESENTATION_REPRESENTATION (  '', ( #20325 ), #12076 ) ;
#12803 = VERTEX_POINT ( 'NONE', #18552 ) ;
#12804 = AXIS2_PLACEMENT_3D ( 'NONE', #7240, #12522, #9036 ) ;
#12805 = CARTESIAN_POINT ( 'NONE',  ( 14.60728983664449387, 19.38727400458104455, -216.6381802409380555 ) ) ;
#12806 = CARTESIAN_POINT ( 'NONE',  ( -12.96364545172611571, 10.77137376900670063, -221.1208843751685720 ) ) ;
#12807 = CARTESIAN_POINT ( 'NONE',  ( -13.96653539523557619, 20.94398119165846239, -231.8597527081015528 ) ) ;
#12808 = CARTESIAN_POINT ( 'NONE',  ( -20.80379704402785990, -7.385557752804055909, -217.9407440132496845 ) ) ;
#12809 = DIRECTION ( 'NONE',  ( 0.000000000000000000, -1.000000000000000000, -0.000000000000000000 ) ) ;
#12810 = VERTEX_POINT ( 'NONE', #3119 ) ;
#12811 = CARTESIAN_POINT ( 'NONE',  ( -14.29986196492902550, 0.06805469746732484282, -227.4167624117703213 ) ) ;
#12812 = CARTESIAN_POINT ( 'NONE',  ( -6.241914139598351952, -12.26321662989467320, -220.9276712261616353 ) ) ;
#12813 = CARTESIAN_POINT ( 'NONE',  ( 20.34032485158648029, 2.741617426884598530, -217.9827731991294968 ) ) ;
#12814 = CARTESIAN_POINT ( 'NONE',  ( -7.825349071214003693, 24.14595706726266755, -216.5959661901539732 ) ) ;
#12815 = CARTESIAN_POINT ( 'NONE',  ( 0.000000000000000000, 0.000000000000000000, 78.50000000000000000 ) ) ;
#12816 = CIRCLE ( 'NONE', #13540, 4.500000000000000888 ) ;
#12817 = CARTESIAN_POINT ( 'NONE',  ( -15.51814470728089645, 2.949994979016113739, -222.8331727603033130 ) ) ;
#12818 = CARTESIAN_POINT ( 'NONE',  ( 18.69149182921226782, 24.00661454656289706, -229.8257469855424517 ) ) ;
#12819 = CARTESIAN_POINT ( 'NONE',  ( 17.68508104102419409, 23.41266195669770767, -227.5327139115408954 ) ) ;
#12820 = LINE ( 'NONE', #4581, #9485 ) ;
#12821 = CARTESIAN_POINT ( 'NONE',  ( -12.37311134093142506, -6.729359123088276995, -218.5215259163429380 ) ) ;
#12822 = CARTESIAN_POINT ( 'NONE',  ( -11.40116373163465369, -15.95513543764466213, -216.7841692646331353 ) ) ;
#12823 = CARTESIAN_POINT ( 'NONE',  ( 7.021536848793814123, -14.49751826649810482, -218.4909385705359455 ) ) ;
#12824 = CARTESIAN_POINT ( 'NONE',  ( -23.00000000000007461, -0.6697502447017975591, -10.00000000000000000 ) ) ;
#12825 = DIRECTION ( 'NONE',  ( 0.000000000000000000, 0.000000000000000000, -1.000000000000000000 ) ) ;
#12826 = CARTESIAN_POINT ( 'NONE',  ( -11.19105919052231179, 21.17456633634251872, -216.2128528132037957 ) ) ;
#12827 = CARTESIAN_POINT ( 'NONE',  ( 13.86864723624500328, -7.301706307425273046, -233.2436966314882909 ) ) ;
#12828 = CARTESIAN_POINT ( 'NONE',  ( 25.54997870115619207, -2.097555195297153841, -218.7002440566220400 ) ) ;
#12829 = CARTESIAN_POINT ( 'NONE',  ( -13.37045227479810094, 5.250293981428504786, -224.2914120185227205 ) ) ;
#12830 = CARTESIAN_POINT ( 'NONE',  ( 7.018811797190238622, 13.93862807232938472, -230.2855929063610176 ) ) ;
#12831 = CARTESIAN_POINT ( 'NONE',  ( 9.653903571287008489, 19.16609876806546353, -219.1149796918802792 ) ) ;
#12832 = EDGE_LOOP ( 'NONE', ( #20894, #17316, #3595, #651, #3378, #4676 ) ) ;
#12833 = CARTESIAN_POINT ( 'NONE',  ( 7.462112298232926655, -14.04285870004232528, -232.2430251799377174 ) ) ;
#12834 = CARTESIAN_POINT ( 'NONE',  ( -9.635142796197669668, 10.84906991693322986, 93.00000000000001421 ) ) ;
#12835 = CARTESIAN_POINT ( 'NONE',  ( -9.578110717394128670, 23.64032677849093034, -215.7669555765890550 ) ) ;
#12836 = CARTESIAN_POINT ( 'NONE',  ( -14.30586181932858914, 18.69563132175512266, -215.8217153853723573 ) ) ;
#12837 = CARTESIAN_POINT ( 'NONE',  ( -12.18037021406049547, -6.685450889859271051, -226.7642181357440734 ) ) ;
#12838 = CARTESIAN_POINT ( 'NONE',  ( -11.02345917017863464, 29.02019856777526741, -223.9475008740665771 ) ) ;
#12839 = CARTESIAN_POINT ( 'NONE',  ( -21.08008464085897060, -0.9048411197481797119, -217.0000000010748522 ) ) ;
#12840 = ADVANCED_FACE ( 'NONE', ( #8310 ), #17057, .F. ) ;
#12841 = CARTESIAN_POINT ( 'NONE',  ( 28.36095019830170472, -8.296631283839911220, -225.2861439608085448 ) ) ;
#12842 = CARTESIAN_POINT ( 'NONE',  ( -2.121548062149551495, 13.26065194155116345, -221.8830439064491884 ) ) ;
#12843 = CARTESIAN_POINT ( 'NONE',  ( -20.67624351032310059, -0.8683020119106035217, -219.0957770725675005 ) ) ;
#12844 = CARTESIAN_POINT ( 'NONE',  ( -28.13472254077564116, 12.33996625515159629, -224.9141344439281909 ) ) ;
#12845 = CARTESIAN_POINT ( 'NONE',  ( 18.04365516558436866, 6.721233635139160612, -218.4376093631473168 ) ) ;
#12846 = DIRECTION ( 'NONE',  ( 1.000000000000000000, -1.083936797661035110E-15, 0.000000000000000000 ) ) ;
#12847 = ADVANCED_FACE ( 'NONE', ( #15294 ), #14192, .F. ) ;
#12848 = CARTESIAN_POINT ( 'NONE',  ( -9.290933312444883185, 29.15551353946876745, -225.8551562993724247 ) ) ;
#12849 = CARTESIAN_POINT ( 'NONE',  ( -23.54665576872953636, -14.78900941482413067, -230.7594827126482073 ) ) ;
#12850 = CARTESIAN_POINT ( 'NONE',  ( 20.41153371889344825, 17.18812948447019551, -230.7531656956970778 ) ) ;
#12851 = CARTESIAN_POINT ( 'NONE',  ( -7.913663017152074097, -13.07021161337726944, -228.8713148165744258 ) ) ;
#12852 = CARTESIAN_POINT ( 'NONE',  ( 1.322875655532295358, 1.500000000000000000, -378.2244600276337678 ) ) ;
#12853 = CARTESIAN_POINT ( 'NONE',  ( -26.38808873681881906, 13.30696350521622939, -225.1492950792419663 ) ) ;
#12854 = CARTESIAN_POINT ( 'NONE',  ( 15.69671663880151868, -19.77919342852767315, -217.9503656454650411 ) ) ;
#12855 = CARTESIAN_POINT ( 'NONE',  ( 5.688640247940316641, 20.34961083808282822, -230.9155060479073711 ) ) ;
#12856 = CARTESIAN_POINT ( 'NONE',  ( -17.49393085256189906, 10.63366922396483361, -217.7502683347138657 ) ) ;
#12857 = CARTESIAN_POINT ( 'NONE',  ( -21.73153953336191790, 8.758376218440917071, -235.2971293019126051 ) ) ;
#12858 = CARTESIAN_POINT ( 'NONE',  ( -5.234434610370643171, -17.78654814248861626, -233.1081320952062867 ) ) ;
#12859 = CARTESIAN_POINT ( 'NONE',  ( 13.72784977962315267, 2.687686193488206143, -220.8507880271885995 ) ) ;
#12860 = DIRECTION ( 'NONE',  ( 1.000000000000000000, 0.000000000000000000, 0.000000000000000000 ) ) ;
#12861 = CARTESIAN_POINT ( 'NONE',  ( -12.06899374386015644, -4.263779665926158202, -221.6855044605631520 ) ) ;
#12862 = CARTESIAN_POINT ( 'NONE',  ( -0.9249541874382023465, 14.55235618511626328, -223.7321818898853962 ) ) ;
#12863 = CARTESIAN_POINT ( 'NONE',  ( 20.05202556141620107, 8.012988804822112954, -215.8722494878839200 ) ) ;
#12864 = CARTESIAN_POINT ( 'NONE',  ( -12.66290653391502907, 23.44312233264792411, -230.9359094203250606 ) ) ;
#12865 = CARTESIAN_POINT ( 'NONE',  ( 6.839751633953758514, 19.11639828585652623, -235.1218211620789873 ) ) ;
#12866 = CARTESIAN_POINT ( 'NONE',  ( -2.821634405314548566, -24.60373223977012458, -232.0829149086248435 ) ) ;
#12867 = CARTESIAN_POINT ( 'NONE',  ( 1.366658787427950772, -15.59113167952139456, -228.2894046839634257 ) ) ;
#12868 = CARTESIAN_POINT ( 'NONE',  ( 18.06016678184731461, 2.257982981100609354, -218.9983079406065940 ) ) ;
#12869 = CARTESIAN_POINT ( 'NONE',  ( 18.55298002304457228, -12.22359628793950570, -216.9137843736221782 ) ) ;
#12870 = CARTESIAN_POINT ( 'NONE',  ( -15.51091956967506391, -1.782849713491490018, -228.8089183834494520 ) ) ;
#12871 = CARTESIAN_POINT ( 'NONE',  ( -9.078153229956912540, -10.71731945587431056, -228.5228069477245469 ) ) ;
#12872 = CARTESIAN_POINT ( 'NONE',  ( 15.03112630398312177, 24.11065413595933293, -226.8236212149936080 ) ) ;
#12873 = CARTESIAN_POINT ( 'NONE',  ( -23.49520248890869212, 11.82830312093803649, -233.3871405502527807 ) ) ;
#12874 = CARTESIAN_POINT ( 'NONE',  ( 4.883314309504700468, 19.06839645569368358, -217.0171359871271193 ) ) ;
#12875 = CARTESIAN_POINT ( 'NONE',  ( 4.152856881432678726, 16.71326706899027670, -228.3712188091315909 ) ) ;
#12876 = CARTESIAN_POINT ( 'NONE',  ( 30.21546680466445167, 0.1681144524405517038, -223.7059097242262737 ) ) ;
#12877 = ORIENTED_EDGE ( 'NONE', *, *, #19590, .T. ) ;
#12878 = CARTESIAN_POINT ( 'NONE',  ( 17.29648694364601980, 10.20782262162153842, -233.8400727604031317 ) ) ;
#12879 = CARTESIAN_POINT ( 'NONE',  ( -13.23768812067001477, 12.78288831771969569, -230.4179793829127902 ) ) ;
#12880 = CARTESIAN_POINT ( 'NONE',  ( -28.00010259152825398, 3.831607968041374157, -225.8381323513402208 ) ) ;
#12881 = CARTESIAN_POINT ( 'NONE',  ( -5.139154528335864391, -14.05392405596956529, -226.2842807754188641 ) ) ;
#12882 = FACE_OUTER_BOUND ( 'NONE', #6242, .T. ) ;
#12883 = CARTESIAN_POINT ( 'NONE',  ( 0.000000000000000000, 0.000000000000000000, 77.51594804401857175 ) ) ;
#12884 = CARTESIAN_POINT ( 'NONE',  ( 2.008896548638861024, 20.64812324442097591, -233.5818019448501843 ) ) ;
#12885 = CARTESIAN_POINT ( 'NONE',  ( 14.64841443880303373, -15.14843974207636101, -218.3573740752273125 ) ) ;
#12886 = CARTESIAN_POINT ( 'NONE',  ( 13.12488928717151637, 1.607335365469798272E-15, -99.99999999999998579 ) ) ;
#12887 = AXIS2_PLACEMENT_3D ( 'NONE', #12452, #20759, #19301 ) ;
#12888 = CARTESIAN_POINT ( 'NONE',  ( -13.60146639818222702, -25.11808310587244009, -230.9974232610874196 ) ) ;
#12889 = APPLICATION_CONTEXT ( 'automotive_design' ) ;
#12890 = SHAPE_DEFINITION_REPRESENTATION ( #20353, #6134 ) ;
#12891 = CARTESIAN_POINT ( 'NONE',  ( 5.141746912158045468, 22.01688500372448232, -216.6678693612369386 ) ) ;
#12892 = CARTESIAN_POINT ( 'NONE',  ( 1.920320557106582893, 25.99317453242502296, -234.5637964893073217 ) ) ;
#12893 = VERTEX_POINT ( 'NONE', #9999 ) ;
#12894 = CARTESIAN_POINT ( 'NONE',  ( -15.58461825850822180, 18.91734573546571951, -233.7691177939990723 ) ) ;
#12895 = CARTESIAN_POINT ( 'NONE',  ( -30.71739798481564421, -2.702902032605977389, -225.9472362185736642 ) ) ;
#12896 = CARTESIAN_POINT ( 'NONE',  ( 28.19769730429874599, -1.268543021275377658, -231.5188709829604363 ) ) ;
#12897 = CARTESIAN_POINT ( 'NONE',  ( -22.44443515611089168, 5.033198366023263759, -8.647132211342501762 ) ) ;
#12898 = EDGE_CURVE ( 'NONE', #20089, #3205, #10579, .T. ) ;
#12899 = CARTESIAN_POINT ( 'NONE',  ( -11.42613629117093765, 28.09170287990588832, -228.7150250545069241 ) ) ;
#12900 = CARTESIAN_POINT ( 'NONE',  ( -20.50691009226094863, -22.90269851828495007, -230.6242067303112435 ) ) ;
#12901 = CARTESIAN_POINT ( 'NONE',  ( 13.82188917133564132, -5.740199443570373816, -227.9076376976435654 ) ) ;
#12902 = CARTESIAN_POINT ( 'NONE',  ( -12.74846050492543625, 19.93509882904884734, -216.0172840992881049 ) ) ;
#12903 = CARTESIAN_POINT ( 'NONE',  ( -13.84508897751235246, 5.904954704487344941, -218.7722818424232401 ) ) ;
#12904 = CARTESIAN_POINT ( 'NONE',  ( 0.3355639943343493026, 23.87279439325363128, -218.0067922387550823 ) ) ;
#12905 = CARTESIAN_POINT ( 'NONE',  ( 0.000000000000000000, 0.000000000000000000, -30.00000000000000000 ) ) ;
#12906 = CARTESIAN_POINT ( 'NONE',  ( 20.41968681625622040, 10.18377600976054076, -218.1989382652844256 ) ) ;
#12907 = CARTESIAN_POINT ( 'NONE',  ( -16.83358080157556103, -19.16169236771116857, -229.6922051654298116 ) ) ;
#12908 = EDGE_LOOP ( 'NONE', ( #11338, #18205, #12094, #16151 ) ) ;
#12909 = CARTESIAN_POINT ( 'NONE',  ( 16.10596270516584028, 24.75152718569329835, -228.9330127594856492 ) ) ;
#12910 = CARTESIAN_POINT ( 'NONE',  ( -14.46024998630872282, 14.54669730493860946, -231.4156670963686508 ) ) ;
#12911 = CARTESIAN_POINT ( 'NONE',  ( -15.57505478537380306, 24.84242291948262249, -225.5907943047649837 ) ) ;
#12912 = VERTEX_POINT ( 'NONE', #1664 ) ;
#12913 = CARTESIAN_POINT ( 'NONE',  ( 27.12528000378512871, -1.050705938820645224, -232.4139529590446784 ) ) ;
#12914 = CARTESIAN_POINT ( 'NONE',  ( -10.76794919243112325, 0.000000000000000000, 95.00000000000000000 ) ) ;
#12915 = ORIENTED_EDGE ( 'NONE', *, *, #4139, .F. ) ;
#12916 = CARTESIAN_POINT ( 'NONE',  ( -13.98136146596813845, 3.850743984385103680, -228.7620665878280590 ) ) ;
#12917 = CARTESIAN_POINT ( 'NONE',  ( -12.16163208632051784, -17.84934472108236747, -234.2417547270719638 ) ) ;
#12918 = CARTESIAN_POINT ( 'NONE',  ( 14.22574309452842733, 4.476723532073429546, -225.5862451792618231 ) ) ;
#12919 = CARTESIAN_POINT ( 'NONE',  ( -2.208416658185406334, 29.10348627872611615, -219.8480645685746424 ) ) ;
#12920 = CARTESIAN_POINT ( 'NONE',  ( 0.000000000000000000, 0.000000000000000000, 90.00000000000000000 ) ) ;
#12921 = CARTESIAN_POINT ( 'NONE',  ( -17.65933056022148762, 0.7424667221540405260, -229.0964312085266386 ) ) ;
#12922 = CARTESIAN_POINT ( 'NONE',  ( 13.06625079052675531, 10.14096931681969238, -232.1435240729728093 ) ) ;
#12923 = CARTESIAN_POINT ( 'NONE',  ( 2.465190328815661892E-29, 24.63401512838760610, 77.51594804401857175 ) ) ;
#12924 = ADVANCED_FACE ( 'NONE', ( #8091 ), #13779, .F. ) ;
#12925 = CARTESIAN_POINT ( 'NONE',  ( 17.43816562714825125, 15.15720016074785903, -232.3748236813696906 ) ) ;
#12926 = CYLINDRICAL_SURFACE ( 'NONE', #15592, 20.99999999999999645 ) ;
#12927 = CARTESIAN_POINT ( 'NONE',  ( 22.78751929883380356, -1.647884454956899836, -231.3901500139513416 ) ) ;
#12928 = CARTESIAN_POINT ( 'NONE',  ( -18.75993824683981970, -9.028840681436806292, -217.1556094966459227 ) ) ;
#12929 = DIRECTION ( 'NONE',  ( -0.000000000000000000, -0.000000000000000000, 1.000000000000000000 ) ) ;
#12930 = CARTESIAN_POINT ( 'NONE',  ( 1.232595164407830946E-29, -17.50000000000007105, -55.00000000000000000 ) ) ;
#12931 = CARTESIAN_POINT ( 'NONE',  ( -1.268862717067444024, 15.25222216985846480, -229.0661283592426116 ) ) ;
#12932 = CARTESIAN_POINT ( 'NONE',  ( 28.41126862162173694, -7.739794849403359933, -232.1728475156252500 ) ) ;
#12933 = CARTESIAN_POINT ( 'NONE',  ( 19.06212547406409641, -9.287000003594721775, -232.7453815625877667 ) ) ;
#12934 = CARTESIAN_POINT ( 'NONE',  ( -24.18895665211001500, 11.26087434487096139, -231.0040666710689550 ) ) ;
#12935 = CARTESIAN_POINT ( 'NONE',  ( 11.96568375430165254, 8.504117401580989721, -219.8633768076029753 ) ) ;
#12936 = CARTESIAN_POINT ( 'NONE',  ( 13.55451907249704213, 16.71566520821242818, -219.1474322952048226 ) ) ;
#12937 = ORIENTED_EDGE ( 'NONE', *, *, #16303, .F. ) ;
#12938 = CARTESIAN_POINT ( 'NONE',  ( 1.038689920556553847, -18.98022482494055652, -217.9213632692622866 ) ) ;
#12939 = DIRECTION ( 'NONE',  ( 0.000000000000000000, 0.000000000000000000, 1.000000000000000000 ) ) ;
#12940 = CARTESIAN_POINT ( 'NONE',  ( 4.719925043692215993, 22.16918918211828782, -214.6883144083888908 ) ) ;
#12941 = CARTESIAN_POINT ( 'NONE',  ( -4.154119475380428916, 11.54776298361823095, -227.0876712548254943 ) ) ;
#12942 = CARTESIAN_POINT ( 'NONE',  ( 20.08508968036338871, -9.819972662663129626, -218.2881406113160381 ) ) ;
#12943 = CARTESIAN_POINT ( 'NONE',  ( -2.808235066048971440, 30.42019778760651150, -222.6481917607299295 ) ) ;
#12944 = CARTESIAN_POINT ( 'NONE',  ( 10.16457016735504304, -10.34237653894239983, 93.00000000000000000 ) ) ;
#12945 =( NAMED_UNIT ( * ) PLANE_ANGLE_UNIT ( ) SI_UNIT ( $, .RADIAN. ) );
#12946 = CARTESIAN_POINT ( 'NONE',  ( -3.712761995161701911, 23.50704853188985766, -216.1220552374512067 ) ) ;
#12947 = CARTESIAN_POINT ( 'NONE',  ( -17.59913672443795463, -0.5356773789333074687, -220.7342471185320960 ) ) ;
#12948 = EDGE_CURVE ( 'NONE', #7956, #3572, #13175, .T. ) ;
#12949 = CARTESIAN_POINT ( 'NONE',  ( -9.250876228778270871, 9.538614635316015722, -227.1332118982684563 ) ) ;
#12950 = CARTESIAN_POINT ( 'NONE',  ( 14.85123888640019452, 5.067529763532427012, -221.9058491819374979 ) ) ;
#12951 = CARTESIAN_POINT ( 'NONE',  ( -5.589224416770360193, 14.13652937339764115, -225.1481999119820330 ) ) ;
#12952 = LINE ( 'NONE', #21262, #21268 ) ;
#12953 = CARTESIAN_POINT ( 'NONE',  ( 2.085064686336211892, 14.99578618537741548, -226.0985834012817861 ) ) ;
#12954 = CARTESIAN_POINT ( 'NONE',  ( -25.10035252441274167, -15.33546242866430198, -228.3913311683031964 ) ) ;
#12955 = CARTESIAN_POINT ( 'NONE',  ( 14.22574309452842733, 4.476723532073429546, -225.5862451792618231 ) ) ;
#12956 = CARTESIAN_POINT ( 'NONE',  ( -5.646690751453034451, -19.25001164140187981, -233.5706237494638913 ) ) ;
#12957 = CARTESIAN_POINT ( 'NONE',  ( 19.02418198972967289, 2.774848290581965582, -223.8390704070222910 ) ) ;
#12958 = EDGE_CURVE ( 'NONE', #12371, #566, #15068, .T. ) ;
#12959 = CARTESIAN_POINT ( 'NONE',  ( -17.99720854823001659, 13.97888873227035056, -232.2992184661552244 ) ) ;
#12960 = CARTESIAN_POINT ( 'NONE',  ( 19.78534257568999166, -22.00365353819481840, -227.2618024355658974 ) ) ;
#12961 = CARTESIAN_POINT ( 'NONE',  ( 6.295505112925526170, 15.36201163567862693, -221.5772643759389098 ) ) ;
#12962 = CARTESIAN_POINT ( 'NONE',  ( -9.988594796049140356, 11.34066464990972811, -226.6453149279956563 ) ) ;
#12963 = CARTESIAN_POINT ( 'NONE',  ( -14.74212732455322161, 0.2624230007780231633, -231.8143822214177874 ) ) ;
#12964 = CARTESIAN_POINT ( 'NONE',  ( -17.58891219272264905, -6.833323493373833379, -229.9407564095759540 ) ) ;
#12965 = CARTESIAN_POINT ( 'NONE',  ( 13.49694890958685711, 2.186465430673721677, -228.8273158381700512 ) ) ;
#12966 = DIRECTION ( 'NONE',  ( -1.000000000000000000, 0.000000000000000000, 0.000000000000000000 ) ) ;
#12967 = CARTESIAN_POINT ( 'NONE',  ( -14.64285150619984677, -17.93374633926643824, -235.3168067477300838 ) ) ;
#12968 = CARTESIAN_POINT ( 'NONE',  ( 0.1556102272723409452, 19.71550568250159685, -232.1993058477363547 ) ) ;
#12969 = CARTESIAN_POINT ( 'NONE',  ( 13.10956039622986324, 4.581323766968698585, -221.0328522389722252 ) ) ;
#12970 = CARTESIAN_POINT ( 'NONE',  ( -16.45414350258782221, 17.57852913985137988, -231.3969631806205598 ) ) ;
#12971 = CARTESIAN_POINT ( 'NONE',  ( 18.69149182921226782, 24.00661454656289706, -229.8257469855424517 ) ) ;
#12972 = CARTESIAN_POINT ( 'NONE',  ( 3.608972370552595343, -15.05750810295313435, -224.7555151483228713 ) ) ;
#12973 = CARTESIAN_POINT ( 'NONE',  ( -2.609511328024065602, -16.97143768612226822, -230.2205646068415490 ) ) ;
#12974 = CARTESIAN_POINT ( 'NONE',  ( 28.57344184061583192, 5.631897254180425527, -225.1192013637692355 ) ) ;
#12975 = CARTESIAN_POINT ( 'NONE',  ( 22.44368505003003378, -11.72633196808685163, -232.1179326287041533 ) ) ;
#12976 = CARTESIAN_POINT ( 'NONE',  ( -28.18501077041064562, -8.523171531337160545, -227.0531053546762337 ) ) ;
#12977 = CARTESIAN_POINT ( 'NONE',  ( -11.88525712185471050, -8.925198460467992589, -221.0951487055306472 ) ) ;
#12978 = CARTESIAN_POINT ( 'NONE',  ( 15.28499842775873319, 22.98894588155567931, -221.0942409093412095 ) ) ;
#12979 = DIRECTION ( 'NONE',  ( -1.000000000000000000, 0.000000000000000000, 0.000000000000000000 ) ) ;
#12980 = CARTESIAN_POINT ( 'NONE',  ( -17.18633058961025029, 6.481319267413964802, -216.1357216783315494 ) ) ;
#12981 = CARTESIAN_POINT ( 'NONE',  ( -3.855805549595750392, 26.68244055262801950, -232.4569730455296508 ) ) ;
#12982 = CARTESIAN_POINT ( 'NONE',  ( -2.532302712337851425, 16.54370602006230939, -228.1940632970506613 ) ) ;
#12983 = CARTESIAN_POINT ( 'NONE',  ( 21.68440970896747544, -13.87065835575754846, -215.6285083892243790 ) ) ;
#12984 = CARTESIAN_POINT ( 'NONE',  ( 21.38922145650625239, 17.10616209967719215, -217.8354246241890451 ) ) ;
#12985 = CARTESIAN_POINT ( 'NONE',  ( -19.72392517715239535, 13.50888179936880107, -230.7714862421596251 ) ) ;
#12986 = CARTESIAN_POINT ( 'NONE',  ( -15.10945752141584464, 6.470132813599071220, -220.1568141593501764 ) ) ;
#12987 = CARTESIAN_POINT ( 'NONE',  ( -1.827935560680505445, -14.81092009092713369, -225.7372845858837707 ) ) ;
#12988 = DIRECTION ( 'NONE',  ( -1.000000000000000000, 0.000000000000000000, 0.000000000000000000 ) ) ;
#12989 = DIRECTION ( 'NONE',  ( 0.000000000000000000, 0.000000000000000000, 1.000000000000000000 ) ) ;
#12990 = CARTESIAN_POINT ( 'NONE',  ( 19.19288224840068935, 10.13059690604263174, -232.1906135022504998 ) ) ;
#12991 = CARTESIAN_POINT ( 'NONE',  ( 16.16137015560671131, -6.751010448487875237, -221.3181884246570519 ) ) ;
#12992 = CARTESIAN_POINT ( 'NONE',  ( -21.43408368508570305, 3.680162304907783621, -233.1134812316964542 ) ) ;
#12993 = EDGE_CURVE ( 'NONE', #7880, #19741, #199, .T. ) ;
#12994 = CARTESIAN_POINT ( 'NONE',  ( -14.34280792637948743, -22.10828917559366147, -217.4172704053049756 ) ) ;
#12995 = APPLICATION_PROTOCOL_DEFINITION ( 'draft international standard', 'automotive_design', 1998, #18778 ) ;
#12996 = EDGE_CURVE ( 'NONE', #3760, #20454, #5135, .T. ) ;
#12997 = CARTESIAN_POINT ( 'NONE',  ( 3.763426558366607111, 28.60172112197566818, -230.1816715025297526 ) ) ;
#12998 = AXIS2_PLACEMENT_3D ( 'NONE', #16483, #13217, #19952 ) ;
#12999 = CARTESIAN_POINT ( 'NONE',  ( -5.568057711815838751, 28.69723585065299076, -232.1518503103610271 ) ) ;
#13000 = VERTEX_POINT ( 'NONE', #1988 ) ;
#13001 = CARTESIAN_POINT ( 'NONE',  ( -7.913358619554302642, 16.16796202616373890, -233.0981776325470491 ) ) ;
#13002 = CARTESIAN_POINT ( 'NONE',  ( -13.63272521699743756, -3.226083955879493814, -228.1383267723209656 ) ) ;
#13003 = CARTESIAN_POINT ( 'NONE',  ( -21.80000000000008242, 0.000000000000000000, -78.50000000000000000 ) ) ;
#13004 = CARTESIAN_POINT ( 'NONE',  ( -20.75208159527516472, 9.917280711861716114, 1.325952641556472189 ) ) ;
#13005 = CARTESIAN_POINT ( 'NONE',  ( -6.571166997218196748, 12.74865329367398736, -229.9840124400968762 ) ) ;
#13006 = CARTESIAN_POINT ( 'NONE',  ( -7.625346832407194242, -11.41809035428902064, -218.7189489878062716 ) ) ;
#13007 = CARTESIAN_POINT ( 'NONE',  ( 13.62757736989142465, -5.584028114184929947, -227.2616851496390211 ) ) ;
#13008 = CARTESIAN_POINT ( 'NONE',  ( -14.07917727715460821, 7.534853284453274291, -218.6337090155677458 ) ) ;
#13009 = TOROIDAL_SURFACE ( 'NONE', #7621, 22.63401512838748175, 3.000000000000002665 ) ;
#13010 = CARTESIAN_POINT ( 'NONE',  ( -14.83095329101371540, 1.580869236763225549, -217.8331819987577660 ) ) ;
#13011 = ORIENTED_EDGE ( 'NONE', *, *, #17601, .F. ) ;
#13012 = CARTESIAN_POINT ( 'NONE',  ( 2.601379523478754674, 17.36677895276155681, -230.4357129074444117 ) ) ;
#13013 = DIRECTION ( 'NONE',  ( 0.000000000000000000, 0.000000000000000000, 1.000000000000000000 ) ) ;
#13014 = CARTESIAN_POINT ( 'NONE',  ( 15.58465056415575312, 2.812367138262562349, -229.5090343034091234 ) ) ;
#13015 = CARTESIAN_POINT ( 'NONE',  ( -7.719684133369767665, -19.28933804209621528, -218.9187502689394478 ) ) ;
#13016 = ORIENTED_EDGE ( 'NONE', *, *, #16549, .T. ) ;
#13017 = CARTESIAN_POINT ( 'NONE',  ( -12.05423124486310904, 12.38527783110887803, -219.7419643105747014 ) ) ;
#13018 = CARTESIAN_POINT ( 'NONE',  ( 11.43247012502872728, 12.44034019618676190, -231.9336559008378629 ) ) ;
#13019 = CARTESIAN_POINT ( 'NONE',  ( 5.030854775705693172, 19.94152319263364603, -234.9034581965229336 ) ) ;
#13020 = AXIS2_PLACEMENT_3D ( 'NONE', #15996, #16438, #16213 ) ;
#13021 = CARTESIAN_POINT ( 'NONE',  ( 30.05917755080113096, -2.930701380670650114, -221.3976229872638726 ) ) ;
#13022 = DIRECTION ( 'NONE',  ( 0.000000000000000000, -1.000000000000000000, 0.000000000000000000 ) ) ;
#13023 = ORIENTED_EDGE ( 'NONE', *, *, #12898, .F. ) ;
#13024 = CARTESIAN_POINT ( 'NONE',  ( -11.98736441306973077, 11.45674391201457176, -217.8252237716743025 ) ) ;
#13025 = CARTESIAN_POINT ( 'NONE',  ( -16.91104737563547644, -22.20641354538343748, -232.3619262256263482 ) ) ;
#13026 = CARTESIAN_POINT ( 'NONE',  ( 28.02123297569005089, 5.903198806000402143, -227.5759114383273811 ) ) ;
#13027 = CARTESIAN_POINT ( 'NONE',  ( 9.107417252317809186, 16.30291009569977234, -218.0131178633739921 ) ) ;
#13028 = CARTESIAN_POINT ( 'NONE',  ( 14.87721638700776694, -2.584478279266595013, -226.5265678059390666 ) ) ;
#13029 = UNCERTAINTY_MEASURE_WITH_UNIT (LENGTH_MEASURE( 1.000000000000000082E-05 ), #16011, 'distance_accuracy_value', 'NONE');
#13030 = CARTESIAN_POINT ( 'NONE',  ( -21.93223149637851677, 1.726402211042445067, -231.1052103444381203 ) ) ;
#13031 = CARTESIAN_POINT ( 'NONE',  ( 21.92281339924938877, 16.67475415235398017, -231.9828670874568957 ) ) ;
#13032 =( NAMED_UNIT ( * ) PLANE_ANGLE_UNIT ( ) SI_UNIT ( $, .RADIAN. ) );
#13033 = AXIS2_PLACEMENT_3D ( 'NONE', #7762, #4147, #11133 ) ;
#13034 = CARTESIAN_POINT ( 'NONE',  ( -24.79131200319441319, 3.238905045468998267, -9.466624808433273586 ) ) ;
#13035 = CARTESIAN_POINT ( 'NONE',  ( 18.04365516558436866, 6.721233635139160612, -218.4376093631473168 ) ) ;
#13036 = CARTESIAN_POINT ( 'NONE',  ( 18.57039993684838564, -7.499893981036622748, -219.4816775992414080 ) ) ;
#13037 = CARTESIAN_POINT ( 'NONE',  ( -11.36971918743327237, -8.287084598727400220, -223.1364763414170227 ) ) ;
#13038 = CARTESIAN_POINT ( 'NONE',  ( 1.526556658859590243E-13, -21.00000000000000000, 75.00000000000000000 ) ) ;
#13039 = EDGE_CURVE ( 'NONE', #15441, #5465, #7292, .T. ) ;
#13040 = CARTESIAN_POINT ( 'NONE',  ( 0.000000000000000000, 0.000000000000000000, -120.0000000000000142 ) ) ;
#13041 = CARTESIAN_POINT ( 'NONE',  ( -2.117958212721558375, 27.20243410318316535, -230.7086725634165418 ) ) ;
#13042 = CARTESIAN_POINT ( 'NONE',  ( 31.06375291838557118, -1.327124779900562768, -220.7315133954257647 ) ) ;
#13043 = CARTESIAN_POINT ( 'NONE',  ( 25.69672030403964769, -15.30292110028031338, -224.0206579222720791 ) ) ;
#13044 = CARTESIAN_POINT ( 'NONE',  ( -12.82737030338386219, 8.595865151885988098, -221.6735325378515142 ) ) ;
#13045 = CARTESIAN_POINT ( 'NONE',  ( 12.25122766587143630, 4.035812653434439845, -225.7709573147497224 ) ) ;
#13046 = CARTESIAN_POINT ( 'NONE',  ( 12.00334754111224100, 12.62951371569041115, -228.5814949098771649 ) ) ;
#13047 = EDGE_LOOP ( 'NONE', ( #5342, #10980, #9197, #15838 ) ) ;
#13048 = CARTESIAN_POINT ( 'NONE',  ( 3.610394173775429039, -14.27701378914486874, -220.9234757326916281 ) ) ;
#13049 = CARTESIAN_POINT ( 'NONE',  ( 3.344898002356376576, 14.20274344593240556, 92.99999999999997158 ) ) ;
#13050 = VECTOR ( 'NONE', #14493, 1000.000000000000000 ) ;
#13051 = CARTESIAN_POINT ( 'NONE',  ( -28.76901170826145560, 13.32870333992657663, -228.6722616467874616 ) ) ;
#13052 = SHAPE_REPRESENTATION ( 'bottom housing_bottom housing', ( #6677 ), #8455 ) ;
#13053 = AXIS2_PLACEMENT_3D ( 'NONE', #10003, #18330, #20751 ) ;
#13054 = CARTESIAN_POINT ( 'NONE',  ( -12.98662328632235585, 28.83726371277012035, -223.5970274767108776 ) ) ;
#13055 = CARTESIAN_POINT ( 'NONE',  ( 5.501756899793208255, 15.97909684020861043, -233.9380718515096191 ) ) ;
#13056 = CARTESIAN_POINT ( 'NONE',  ( 14.02135871364020936, -4.809710560857269002, -224.5109434094503911 ) ) ;
#13057 = CARTESIAN_POINT ( 'NONE',  ( -11.33137429837660193, 27.25022425932026238, -230.1650924901870212 ) ) ;
#13058 = FACE_OUTER_BOUND ( 'NONE', #21179, .T. ) ;
#13059 = CARTESIAN_POINT ( 'NONE',  ( 2.276720224425493821, 13.44951395023989171, -229.9230017221896105 ) ) ;
#13060 = CARTESIAN_POINT ( 'NONE',  ( 26.56239871811266440, 9.439457669498057868, -217.7226690415261885 ) ) ;
#13061 = CARTESIAN_POINT ( 'NONE',  ( -11.98736441306973077, 11.45674391201457176, -217.8252237716743025 ) ) ;
#13062 = CARTESIAN_POINT ( 'NONE',  ( 24.58316096239279602, 5.861425670879941485, -231.3104446318280623 ) ) ;
#13063 = TOROIDAL_SURFACE ( 'NONE', #4776, 22.56777165119825668, 3.000000000000000000 ) ;
#13064 = CARTESIAN_POINT ( 'NONE',  ( 6.173705828530630768, 14.85108299334794957, -222.6284669816953112 ) ) ;
#13065 = CONICAL_SURFACE ( 'NONE', #15951, 25.00000000000000000, 0.1745329251994333364 ) ;
#13066 = DIRECTION ( 'NONE',  ( -1.000000000000000000, 1.224646799147352961E-16, 0.000000000000000000 ) ) ;
#13067 = CARTESIAN_POINT ( 'NONE',  ( 16.01130065545721592, 20.79417322911648114, -220.9619135886794652 ) ) ;
#13068 = CARTESIAN_POINT ( 'NONE',  ( -25.82802808205240552, -14.78441951539553401, -222.6940535085979604 ) ) ;
#13069 = CARTESIAN_POINT ( 'NONE',  ( 13.69275646168278371, 8.674223198772375909, -220.8699857572541987 ) ) ;
#13070 = CARTESIAN_POINT ( 'NONE',  ( -3.168869516962652622, -26.26615012824360207, -217.0152745877844040 ) ) ;
#13071 = DIRECTION ( 'NONE',  ( 1.000000000000000000, 0.000000000000000000, 0.000000000000000000 ) ) ;
#13072 = EDGE_CURVE ( 'NONE', #3572, #722, #4818, .T. ) ;
#13073 = CARTESIAN_POINT ( 'NONE',  ( -7.250603130619442283, 20.89725557392719324, -217.7893896917081520 ) ) ;
#13074 = CARTESIAN_POINT ( 'NONE',  ( 24.14841045621385263, -15.62485098017456586, -229.9279278555176518 ) ) ;
#13075 = CARTESIAN_POINT ( 'NONE',  ( 25.85827166240959940, 13.84420748389600675, -220.2831452073696425 ) ) ;
#13076 = CARTESIAN_POINT ( 'NONE',  ( -12.82737030338386219, 8.595865151885988098, -221.6735325378515142 ) ) ;
#13077 = CARTESIAN_POINT ( 'NONE',  ( -16.95112677453439431, 10.32962960657076934, -214.9445123409346650 ) ) ;
#13078 = CARTESIAN_POINT ( 'NONE',  ( -24.64494147011371084, -8.645298684267959999, -229.1812397229770113 ) ) ;
#13079 = CARTESIAN_POINT ( 'NONE',  ( 22.92330650806121639, 19.11387742755395180, -231.6463539987045976 ) ) ;
#13080 = AXIS2_PLACEMENT_3D ( 'NONE', #1319, #8302, #6487 ) ;
#13081 = CARTESIAN_POINT ( 'NONE',  ( 0.000000000000000000, 0.000000000000000000, -105.0000000000000142 ) ) ;
#13082 = CARTESIAN_POINT ( 'NONE',  ( -19.82723516873631908, -6.367811336401608457, -234.7370909334860869 ) ) ;
#13083 = CARTESIAN_POINT ( 'NONE',  ( 1.939863782649466017, 28.20584428268631783, -229.4487744520996273 ) ) ;
#13084 = CARTESIAN_POINT ( 'NONE',  ( 27.69955354773053458, 12.81264626165819287, -221.7750850138309602 ) ) ;
#13085 = CARTESIAN_POINT ( 'NONE',  ( -11.83954511762131112, 10.58068896997146346, -226.6171226499791089 ) ) ;
#13086 = CARTESIAN_POINT ( 'NONE',  ( 3.714886539878811789, 12.88803176524806560, -219.5889136906770034 ) ) ;
#13087 = VERTEX_POINT ( 'NONE', #14164 ) ;
#13088 = CARTESIAN_POINT ( 'NONE',  ( 0.7938325546108213615, -23.90362011959725663, -218.0438616059182380 ) ) ;
#13089 = CARTESIAN_POINT ( 'NONE',  ( 1.874647746501092893, -15.20125101474619633, -222.7462710229423521 ) ) ;
#13090 = CARTESIAN_POINT ( 'NONE',  ( -12.36382104905844592, -0.1264132474004772688, -228.0034406263598896 ) ) ;
#13091 = CARTESIAN_POINT ( 'NONE',  ( 24.80560757033128993, -15.22139526172250079, -221.3338856610240271 ) ) ;
#13092 = CARTESIAN_POINT ( 'NONE',  ( -25.95884575339096401, -1.972114683626720044, -231.2145524501483749 ) ) ;
#13093 = CARTESIAN_POINT ( 'NONE',  ( -12.42894476027428929, -17.97759322220185396, -216.3110355466728834 ) ) ;
#13094 = CARTESIAN_POINT ( 'NONE',  ( 3.182992543297812560, 16.68308636702302650, -221.9272281984358415 ) ) ;
#13095 = DIRECTION ( 'NONE',  ( 0.000000000000000000, 0.000000000000000000, -1.000000000000000000 ) ) ;
#13096 = CARTESIAN_POINT ( 'NONE',  ( -30.35034897870229287, 7.696526532841741819, -221.5749790623549416 ) ) ;
#13097 = AXIS2_PLACEMENT_3D ( 'NONE', #10635, #22221, #1742 ) ;
#13098 = CARTESIAN_POINT ( 'NONE',  ( 8.979547488457603421, 23.24376652602565230, -232.6628827740196357 ) ) ;
#13099 = CARTESIAN_POINT ( 'NONE',  ( 7.804112641607792611, 19.76858558208418515, -218.6463059509973164 ) ) ;
#13100 = CARTESIAN_POINT ( 'NONE',  ( 9.734612854996214537, -6.789898087979761243, -225.0934417779699004 ) ) ;
#13101 = CARTESIAN_POINT ( 'NONE',  ( 17.31940731551425827, 24.90170669671083914, -222.9868986272316533 ) ) ;
#13102 = CARTESIAN_POINT ( 'NONE',  ( -11.82020046940938407, 10.16362659047642758, -224.3364193436540575 ) ) ;
#13103 = CARTESIAN_POINT ( 'NONE',  ( -16.29666348338687953, 2.994680995215331709, -221.2421885839926006 ) ) ;
#13104 = CARTESIAN_POINT ( 'NONE',  ( 4.002939343642331949, -22.37368820207002429, -217.8631878264377804 ) ) ;
#13105 = DIRECTION ( 'NONE',  ( -2.162300680179986877E-16, -1.000000000000000000, 0.000000000000000000 ) ) ;
#13106 = LINE ( 'NONE', #11306, #73 ) ;
#13107 = CARTESIAN_POINT ( 'NONE',  ( 18.76922974182421555, 13.12635134380198210, -217.8010375391909008 ) ) ;
#13108 = CARTESIAN_POINT ( 'NONE',  ( 10.54788747927062964, -11.30141756528536412, -223.8337882627521651 ) ) ;
#13109 = CARTESIAN_POINT ( 'NONE',  ( -14.07336028695978314, 1.752429266630609828, -222.9750305084206161 ) ) ;
#13110 = ADVANCED_FACE ( 'NONE', ( #10666 ), #18484, .F. ) ;
#13111 = CARTESIAN_POINT ( 'NONE',  ( -8.491902988188710921, -10.37035003683405066, -223.9502466269643435 ) ) ;
#13112 = SHAPE_DEFINITION_REPRESENTATION ( #11932, #5277 ) ;
#13113 = CARTESIAN_POINT ( 'NONE',  ( 4.343013938751969505, 13.02036404005131587, -224.7825435359082178 ) ) ;
#13114 = AXIS2_PLACEMENT_3D ( 'NONE', #7375, #14244, #5664 ) ;
#13115 = CARTESIAN_POINT ( 'NONE',  ( -5.467362224022371819, 23.92882567691090046, -234.7811165710531611 ) ) ;
#13116 = ORIENTED_EDGE ( 'NONE', *, *, #16303, .T. ) ;
#13117 = CARTESIAN_POINT ( 'NONE',  ( -3.855805549595750392, 26.68244055262801950, -232.4569730455296508 ) ) ;
#13118 = CARTESIAN_POINT ( 'NONE',  ( -14.84457943406284208, -4.054717634150219574, -219.4128920803699430 ) ) ;
#13119 = CARTESIAN_POINT ( 'NONE',  ( -23.02481977093860621, -9.739746005238293591, -2.290462534298830288 ) ) ;
#13120 = DIRECTION ( 'NONE',  ( -1.000000000000000000, 0.000000000000000000, 0.000000000000000000 ) ) ;
#13121 = CARTESIAN_POINT ( 'NONE',  ( -13.58874046263339608, 12.73011668665171392, -216.5659449791897941 ) ) ;
#13122 = CARTESIAN_POINT ( 'NONE',  ( -13.27281469842883688, -16.60017218729922561, -235.3541344917538254 ) ) ;
#13123 = CARTESIAN_POINT ( 'NONE',  ( 25.69672030403964769, -15.30292110028031338, -224.0206579222720791 ) ) ;
#13124 = CARTESIAN_POINT ( 'NONE',  ( -3.205260335674071648, 17.52234722004434531, -232.9754319808710363 ) ) ;
#13125 = CARTESIAN_POINT ( 'NONE',  ( -17.18633058961025029, 6.481319267413964802, -216.1357216783315494 ) ) ;
#13126 = EDGE_CURVE ( 'NONE', #22217, #12646, #208, .T. ) ;
#13127 = CARTESIAN_POINT ( 'NONE',  ( -1.470815287892122125, 29.54293232078718745, -224.5855911371830302 ) ) ;
#13128 = FACE_OUTER_BOUND ( 'NONE', #19469, .T. ) ;
#13129 = CARTESIAN_POINT ( 'NONE',  ( 19.31922195716811430, 9.600631919686000160, -218.1359845693048101 ) ) ;
#13130 = CARTESIAN_POINT ( 'NONE',  ( -8.126933673790581736, -26.89509779614531126, -227.4795931708183048 ) ) ;
#13131 = ORIENTED_EDGE ( 'NONE', *, *, #7732, .F. ) ;
#13132 = CARTESIAN_POINT ( 'NONE',  ( -12.87285471141929172, 9.485162256560764504, -229.1865421006261840 ) ) ;
#13133 = CARTESIAN_POINT ( 'NONE',  ( 20.26651059498356844, 18.95255124124090074, -231.7206897233655525 ) ) ;
#13134 = CARTESIAN_POINT ( 'NONE',  ( 2.469769522101480597, 18.85781121334172639, -215.5372409425634430 ) ) ;
#13135 = CARTESIAN_POINT ( 'NONE',  ( -20.79829908948044448, -4.820361304162784855, -232.2223801333801703 ) ) ;
#13136 = EDGE_CURVE ( 'NONE', #2027, #7856, #13741, .T. ) ;
#13137 = VECTOR ( 'NONE', #19558, 1000.000000000000000 ) ;
#13138 = ORIENTED_EDGE ( 'NONE', *, *, #14186, .T. ) ;
#13139 = COLOUR_RGB ( '', 0.72549020, 0.75294118, 0.79215686) ;
#13140 = CARTESIAN_POINT ( 'NONE',  ( -12.44873260470819787, 7.411970124596155785, -229.4214091473984070 ) ) ;
#13141 = CARTESIAN_POINT ( 'NONE',  ( -3.368184987477955694, -15.91886893360235078, -219.1066823976216256 ) ) ;
#13142 = CARTESIAN_POINT ( 'NONE',  ( 0.000000000000000000, 0.000000000000000000, 75.00000000000000000 ) ) ;
#13143 = CARTESIAN_POINT ( 'NONE',  ( 11.13678936984666912, 26.95732789089726111, -228.8350761760834757 ) ) ;
#13144 = DIRECTION ( 'NONE',  ( 0.000000000000000000, 0.000000000000000000, -1.000000000000000000 ) ) ;
#13145 = CARTESIAN_POINT ( 'NONE',  ( -14.58084844870496966, 13.85720943031455832, -233.3219724312919254 ) ) ;
#13146 = CARTESIAN_POINT ( 'NONE',  ( 23.64727379217503866, 9.907944788639682088, -232.0643337313508709 ) ) ;
#13147 = CARTESIAN_POINT ( 'NONE',  ( -24.74863962610228185, 3.549617057581722968, -9.354628607790802519 ) ) ;
#13148 = CARTESIAN_POINT ( 'NONE',  ( 16.64225601860865211, 1.926018578292457928, -220.2177910260893725 ) ) ;
#13149 = CARTESIAN_POINT ( 'NONE',  ( -23.03038449397558196, 2.820408665368003469E-15, 75.34729635533385306 ) ) ;
#13150 = CARTESIAN_POINT ( 'NONE',  ( 25.46431111394153390, -2.048831322092446783, -230.3135391428295975 ) ) ;
#13151 = CARTESIAN_POINT ( 'NONE',  ( -23.10791503177032880, -5.282985115830100220, -217.6364121950018671 ) ) ;
#13152 = PRESENTATION_LAYER_ASSIGNMENT (  '', '', ( #17109 ) ) ;
#13153 = DIRECTION ( 'NONE',  ( 0.000000000000000000, 0.000000000000000000, -1.000000000000000000 ) ) ;
#13154 = CYLINDRICAL_SURFACE ( 'NONE', #471, 17.50000000000000711 ) ;
#13155 = CARTESIAN_POINT ( 'NONE',  ( -14.00980274651940682, 20.05588230486321066, -234.2453272803952586 ) ) ;
#13156 = CARTESIAN_POINT ( 'NONE',  ( 25.79180107113126397, -16.09695083256378112, -231.0225534820104656 ) ) ;
#13157 = CARTESIAN_POINT ( 'NONE',  ( 24.80560757033128993, -15.22139526172250079, -221.3338856610240271 ) ) ;
#13158 = CARTESIAN_POINT ( 'NONE',  ( -25.19248792833826300, 13.40115236862232528, -221.2817950683888455 ) ) ;
#13159 = CARTESIAN_POINT ( 'NONE',  ( -19.67797246974518544, 1.229961341702398681, -219.4743747885323160 ) ) ;
#13160 = CARTESIAN_POINT ( 'NONE',  ( 12.91443243054181700, 13.28840485332751875, -229.6651346406987955 ) ) ;
#13161 = ORIENTED_EDGE ( 'NONE', *, *, #8982, .T. ) ;
#13162 = CARTESIAN_POINT ( 'NONE',  ( -0.6720842648862578317, -17.90033647106004011, -231.4757128331908973 ) ) ;
#13163 = CARTESIAN_POINT ( 'NONE',  ( -11.67815946035152308, 8.814245471595203441, 93.00000000000001421 ) ) ;
#13164 = CARTESIAN_POINT ( 'NONE',  ( -15.57331739480619248, 4.297375044201914740, -216.4079605712025511 ) ) ;
#13165 = CARTESIAN_POINT ( 'NONE',  ( 12.65306858828212810, 29.42930486385247590, -226.3758484992818012 ) ) ;
#13166 = CARTESIAN_POINT ( 'NONE',  ( 1.920320557106582893, 25.99317453242502296, -234.5637964893073217 ) ) ;
#13167 = CARTESIAN_POINT ( 'NONE',  ( 14.09645999499448088, -9.025099991742237648, -228.8994629750086744 ) ) ;
#13168 = CARTESIAN_POINT ( 'NONE',  ( -12.74846050492543625, 19.93509882904884734, -216.0172840992881049 ) ) ;
#13169 = CARTESIAN_POINT ( 'NONE',  ( -29.95012366401462955, 4.746560250930182967, -224.6954343660969471 ) ) ;
#13170 = STYLED_ITEM ( 'NONE', ( #19641 ), #6837 ) ;
#13171 = CARTESIAN_POINT ( 'NONE',  ( 15.89102655998366664, 24.10108298038447572, -232.7733025413564008 ) ) ;
#13172 = CARTESIAN_POINT ( 'NONE',  ( -17.65933056022148762, 0.7424667221540405260, -229.0964312085266386 ) ) ;
#13173 = CARTESIAN_POINT ( 'NONE',  ( -21.02719846458807851, 18.12262440796364871, -218.0220709499931502 ) ) ;
#13174 = CARTESIAN_POINT ( 'NONE',  ( 18.46552355142154411, 5.019711608606525211, -231.5099115070375433 ) ) ;
#13175 = B_SPLINE_CURVE_WITH_KNOTS ( 'NONE', 3,
 ( #20209, #21797, #9998, #15177, #11456, #15293, #6732, #6614, #2885, #3000, #20099, #9883, #1215, #18767, #11902, #18663, #8090, #6383, #20437, #4688, #16747, #1327 ),
 .UNSPECIFIED., .F., .F.,
 ( 4, 2, 2, 2, 2, 2, 2, 2, 2, 2, 4 ),
 ( 0.005800309973861407335, 0.006162931802048039927, 0.006525553630234673386, 0.006888175458421305977, 0.007250797286607938569, 0.007976040942981144771, 0.008701284599354350974, 0.01015177191210072175, 0.01087701556847389672, 0.01123963739666048595, 0.01160225922484707343 ),
 .UNSPECIFIED. ) ;
#13176 = CARTESIAN_POINT ( 'NONE',  ( 7.017641603801325623, 14.96204511409594673, -228.1064041248110073 ) ) ;
#13177 = CARTESIAN_POINT ( 'NONE',  ( 18.00000000000000000, 1.360023205165816762E-13, 0.000000000000000000 ) ) ;
#13178 = DIRECTION ( 'NONE',  ( 1.000000000000000000, 0.000000000000000000, 0.000000000000000000 ) ) ;
#13179 = ADVANCED_FACE ( 'NONE', ( #6841 ), #3056, .F. ) ;
#13180 = CARTESIAN_POINT ( 'NONE',  ( 8.961491954973460849, 17.27041174997091844, -219.7661252763212474 ) ) ;
#13181 = CARTESIAN_POINT ( 'NONE',  ( -17.42499862437977853, -18.98713029041037004, -232.7811807006768845 ) ) ;
#13182 = CARTESIAN_POINT ( 'NONE',  ( 26.48990917286906921, 12.16675355942207659, -225.0153622588060216 ) ) ;
#13183 = CARTESIAN_POINT ( 'NONE',  ( -9.481788909210624894, -22.96916533494018253, -217.3969400264330716 ) ) ;
#13184 = CARTESIAN_POINT ( 'NONE',  ( 21.65362371779454520, 0.3438195010044668432, -222.0185330407754520 ) ) ;
#13185 = CARTESIAN_POINT ( 'NONE',  ( -16.50467377682197423, 21.56569464670658220, -229.9175202103629374 ) ) ;
#13186 = CARTESIAN_POINT ( 'NONE',  ( 11.97732832373273126, -6.576952149368169742, -223.6031523087739572 ) ) ;
#13187 = CARTESIAN_POINT ( 'NONE',  ( 12.23475091788960434, 6.342242864926500800, -221.9572581868331156 ) ) ;
#13188 = CARTESIAN_POINT ( 'NONE',  ( -9.233762381136051189, 19.18161952504991419, -232.0796851897838451 ) ) ;
#13189 = CARTESIAN_POINT ( 'NONE',  ( -13.06407726305387307, 3.888674610242962348, -219.0371145420960204 ) ) ;
#13190 = CARTESIAN_POINT ( 'NONE',  ( -19.94082127283490280, -7.534429669270808816, -230.8553971038493557 ) ) ;
#13191 = CARTESIAN_POINT ( 'NONE',  ( 21.06229272850552547, 3.434461253538921621, -234.1452885155528918 ) ) ;
#13192 = CARTESIAN_POINT ( 'NONE',  ( 0.000000000000000000, -23.00000000000006040, 75.00000000000000000 ) ) ;
#13193 = CARTESIAN_POINT ( 'NONE',  ( -16.32911940539174367, -0.4850290419235887551, -232.0399150213553412 ) ) ;
#13194 = CARTESIAN_POINT ( 'NONE',  ( 14.69879291197755222, 10.86005690695417236, -216.7815908316746913 ) ) ;
#13195 = CARTESIAN_POINT ( 'NONE',  ( 17.22423229049764970, 1.395540479540137380, -217.3898520248025363 ) ) ;
#13196 = CARTESIAN_POINT ( 'NONE',  ( -1.585416880194127520, 15.28258783379090424, -231.0852564988603319 ) ) ;
#13197 = CARTESIAN_POINT ( 'NONE',  ( 9.533850545951205291, 16.09136358716069637, -215.9093469876620475 ) ) ;
#13198 = CARTESIAN_POINT ( 'NONE',  ( 3.191506000329551007, -19.56356538597602679, -231.2193641236077326 ) ) ;
#13199 = EDGE_CURVE ( 'NONE', #15746, #10887, #15665, .T. ) ;
#13200 = EDGE_LOOP ( 'NONE', ( #8907, #9407 ) ) ;
#13201 = CARTESIAN_POINT ( 'NONE',  ( -5.322766963623397629, -16.65786661440869665, -219.3972027188067671 ) ) ;
#13202 = CARTESIAN_POINT ( 'NONE',  ( -12.13319425917249283, 4.024026700415168634, -229.5243363405849095 ) ) ;
#13203 = CARTESIAN_POINT ( 'NONE',  ( 15.05686526350529775, -5.555778903407086133, -220.1433349335996468 ) ) ;
#13204 = CARTESIAN_POINT ( 'NONE',  ( -14.37894460687751597, -1.926260335694933268, -225.0161641904981593 ) ) ;
#13205 = CARTESIAN_POINT ( 'NONE',  ( -12.13177435108894642, -8.392035797555511323, -228.8392847287196332 ) ) ;
#13206 = CARTESIAN_POINT ( 'NONE',  ( 21.24820809707834357, 20.59746639607275398, -225.8540969741923732 ) ) ;
#13207 = SURFACE_SIDE_STYLE ('',( #6000 ) ) ;
#13208 = CARTESIAN_POINT ( 'NONE',  ( -15.33438615632468149, 23.56248205204123991, -229.2747191038674544 ) ) ;
#13209 = CARTESIAN_POINT ( 'NONE',  ( 25.85827166240959940, 13.84420748389600675, -220.2831452073696425 ) ) ;
#13210 = CARTESIAN_POINT ( 'NONE',  ( 11.33210854356620523, 22.81476816607802149, -217.8536224460118262 ) ) ;
#13211 = CARTESIAN_POINT ( 'NONE',  ( 17.98704291748025952, 16.14142602298251461, -217.3684083235702644 ) ) ;
#13212 = CARTESIAN_POINT ( 'NONE',  ( 10.30964016151751750, -15.48526446506176413, -234.8200832677974859 ) ) ;
#13213 = CARTESIAN_POINT ( 'NONE',  ( 13.86383614057800884, 4.939477956453596441, -219.6543243356308324 ) ) ;
#13214 = CARTESIAN_POINT ( 'NONE',  ( -8.900302563431933933, 20.17395648083808268, -216.9116515890487733 ) ) ;
#13215 = CARTESIAN_POINT ( 'NONE',  ( -10.03082531488024109, -22.09229706162428286, -231.9736132431984572 ) ) ;
#13216 = CARTESIAN_POINT ( 'NONE',  ( -16.74550766701807447, 3.787526820511904813, -217.9802846976114381 ) ) ;
#13217 = DIRECTION ( 'NONE',  ( 0.000000000000000000, 0.000000000000000000, 1.000000000000000000 ) ) ;
#13218 = CARTESIAN_POINT ( 'NONE',  ( 21.39553407250273054, 8.453402029343234148, -217.9531594780983141 ) ) ;
#13219 = CARTESIAN_POINT ( 'NONE',  ( 15.01754996320599744, -10.17932250226635738, -220.3401326760229040 ) ) ;
#13220 = CARTESIAN_POINT ( 'NONE',  ( -13.96147744945181124, 5.260363697127891314, -222.3342733685200301 ) ) ;
#13221 = CARTESIAN_POINT ( 'NONE',  ( -7.800954605602409053, -29.95157606033723496, -226.5906573908930000 ) ) ;
#13222 = CARTESIAN_POINT ( 'NONE',  ( -18.94009481283715957, 3.115208415279245191, -230.3622730452590588 ) ) ;
#13223 = CARTESIAN_POINT ( 'NONE',  ( 1.557078628722260438, 24.20011951319323273, -235.1441088220640268 ) ) ;
#13224 = ORIENTED_EDGE ( 'NONE', *, *, #4161, .F. ) ;
#13225 = CARTESIAN_POINT ( 'NONE',  ( -8.501641725227710111, 25.47064987787527102, -217.3358698761548737 ) ) ;
#13226 = CARTESIAN_POINT ( 'NONE',  ( -17.83852468596024110, -8.357198216422425219, -233.0481596892792879 ) ) ;
#13227 = CARTESIAN_POINT ( 'NONE',  ( 30.87761267810551757, -2.376991648450896388, -225.4116222034606949 ) ) ;
#13228 = DIRECTION ( 'NONE',  ( 0.000000000000000000, 0.000000000000000000, -1.000000000000000000 ) ) ;
#13229 = CARTESIAN_POINT ( 'NONE',  ( 5.623554730548537606, 15.65270319720736225, -231.3185741195121068 ) ) ;
#13230 = CARTESIAN_POINT ( 'NONE',  ( -7.108809775916832940, -10.55228017211132929, -220.3225562754048212 ) ) ;
#13231 = CARTESIAN_POINT ( 'NONE',  ( 10.30328786010431052, -20.08430705480546408, -216.1847100135515802 ) ) ;
#13232 = CARTESIAN_POINT ( 'NONE',  ( 13.96958060839473958, -9.488587112651741151, -218.7731372952745232 ) ) ;
#13233 = CARTESIAN_POINT ( 'NONE',  ( -8.221702953833418093, 11.87876791566348800, -223.9138461338794741 ) ) ;
#13234 = CARTESIAN_POINT ( 'NONE',  ( 11.27486163995310164, 25.12851252939060487, -222.6718455410222930 ) ) ;
#13235 = CARTESIAN_POINT ( 'NONE',  ( -28.99926036811508467, 3.909990568804979194, -228.9613767892386988 ) ) ;
#13236 = CARTESIAN_POINT ( 'NONE',  ( -12.89119823113977503, 10.10140484475961564, -218.5945808114896636 ) ) ;
#13237 = CARTESIAN_POINT ( 'NONE',  ( -26.75342641616541783, -10.60804028525731546, -225.2137697103424898 ) ) ;
#13238 = EDGE_CURVE ( 'NONE', #15108, #6126, #4753, .T. ) ;
#13239 = CARTESIAN_POINT ( 'NONE',  ( -22.24722865165759345, 18.77558306771206986, -226.5077042908023941 ) ) ;
#13240 = CARTESIAN_POINT ( 'NONE',  ( 21.52074627118099315, 8.791036694007010155, -215.9547738671300294 ) ) ;
#13241 = CARTESIAN_POINT ( 'NONE',  ( 1.898427734299754421, 12.47096978853034521, -227.5043976727869506 ) ) ;
#13242 = VECTOR ( 'NONE', #13105, 1000.000000000000000 ) ;
#13243 = CARTESIAN_POINT ( 'NONE',  ( -26.24201160508392761, -9.884581200937399004, -221.6903139798603206 ) ) ;
#13244 = EDGE_LOOP ( 'NONE', ( #15492, #12465, #2440, #20565 ) ) ;
#13245 = CARTESIAN_POINT ( 'NONE',  ( -17.65835845419170624, 22.55329142274348442, -231.2673511165784532 ) ) ;
#13246 = CARTESIAN_POINT ( 'NONE',  ( -4.782174899302804150, -29.09898918907212817, -227.3916599557566940 ) ) ;
#13247 = CARTESIAN_POINT ( 'NONE',  ( 28.57344184061583192, 5.631897254180425527, -225.1192013637692355 ) ) ;
#13248 = CARTESIAN_POINT ( 'NONE',  ( 8.979547488457603421, 23.24376652602565230, -232.6628827740196357 ) ) ;
#13249 = FACE_OUTER_BOUND ( 'NONE', #5364, .T. ) ;
#13250 = PRODUCT_DEFINITION_CONTEXT ( 'detailed design', #14059, 'design' ) ;
#13251 = CARTESIAN_POINT ( 'NONE',  ( -11.94727018630768178, 9.025563988971828877, -220.6148682757971358 ) ) ;
#13252 = CARTESIAN_POINT ( 'NONE',  ( 22.37138132874926910, 6.723028048925958622, -217.7073806909121743 ) ) ;
#13253 = FILL_AREA_STYLE_COLOUR ( '', #9525 ) ;
#13254 = CARTESIAN_POINT ( 'NONE',  ( 15.54590875671327233, 1.102094689760376056, -222.2065310083714849 ) ) ;
#13255 = CARTESIAN_POINT ( 'NONE',  ( 18.60971343765040942, 2.368090295052050820, -218.6871071987073094 ) ) ;
#13256 = CIRCLE ( 'NONE', #2471, 17.50000000000007816 ) ;
#13257 = CARTESIAN_POINT ( 'NONE',  ( -25.00000000000000000, 0.000000000000000000, 75.00000000000000000 ) ) ;
#13258 = CARTESIAN_POINT ( 'NONE',  ( 16.24842259479558848, -3.494976385286828080, -222.6392560871376816 ) ) ;
#13259 = CARTESIAN_POINT ( 'NONE',  ( -17.58118739749173898, -8.238107657346720458, -217.5252134542318458 ) ) ;
#13260 = CARTESIAN_POINT ( 'NONE',  ( -23.00000000000000000, -1.421401133463427911E-20, 10.00000000000000000 ) ) ;
#13261 = CARTESIAN_POINT ( 'NONE',  ( -17.50000000000000711, 0.000000000000000000, -60.00000000000000000 ) ) ;
#13262 = CARTESIAN_POINT ( 'NONE',  ( 8.858651440950676914, 22.47383302477780376, -230.7859943773311215 ) ) ;
#13263 = CARTESIAN_POINT ( 'NONE',  ( 13.44856294975069488, -28.16358066815265460, -226.3235907536142406 ) ) ;
#13264 = CARTESIAN_POINT ( 'NONE',  ( 13.91151814069282722, -15.58123622716646572, -216.5183035683795367 ) ) ;
#13265 = CARTESIAN_POINT ( 'NONE',  ( -11.94782396647286049, 8.456988817430419303, -225.5094493096559063 ) ) ;
#13266 = CARTESIAN_POINT ( 'NONE',  ( 21.52074627118099315, 8.791036694007010155, -215.9547738671300294 ) ) ;
#13267 = CARTESIAN_POINT ( 'NONE',  ( 25.53003411612920459, 7.940385729200389875, -230.5495695598654322 ) ) ;
#13268 = ORIENTED_EDGE ( 'NONE', *, *, #2358, .T. ) ;
#13269 = CARTESIAN_POINT ( 'NONE',  ( 13.50228739682142454, -27.74890714798514679, -227.9743917065363519 ) ) ;
#13270 = PLANE ( 'NONE',  #91 ) ;
#13271 = CARTESIAN_POINT ( 'NONE',  ( -16.81617677814535128, 0.6259372974186930838, -233.5115673467681745 ) ) ;
#13272 = CARTESIAN_POINT ( 'NONE',  ( 10.81638188557560731, 14.98959006186633403, -234.2424515599453514 ) ) ;
#13273 = CARTESIAN_POINT ( 'NONE',  ( 3.490345297502855715, 11.17751288514984331, -224.7799703251421022 ) ) ;
#13274 = CARTESIAN_POINT ( 'NONE',  ( 23.21483485987735307, -16.21330837850192097, -225.6840547952056397 ) ) ;
#13275 = CARTESIAN_POINT ( 'NONE',  ( -6.282398543089500187, 12.01615879894893801, -228.5121145169883903 ) ) ;
#13276 = CARTESIAN_POINT ( 'NONE',  ( -13.10651848559790444, 3.262242204071156948, -224.3513854875720597 ) ) ;
#13277 = EDGE_CURVE ( 'NONE', #18650, #1959, #8789, .T. ) ;
#13278 = CARTESIAN_POINT ( 'NONE',  ( 14.82579616070250417, 22.96152595385638762, -233.8920860146931489 ) ) ;
#13279 = CARTESIAN_POINT ( 'NONE',  ( -19.92987771446595957, 11.92619342620000999, -232.5382020162021206 ) ) ;
#13280 = CARTESIAN_POINT ( 'NONE',  ( -2.934221234790329369, 15.07857928364152222, -230.9558365497803720 ) ) ;
#13281 = CARTESIAN_POINT ( 'NONE',  ( 16.84848658399567611, 11.39632653812981644, -217.9589513831453473 ) ) ;
#13282 = CARTESIAN_POINT ( 'NONE',  ( 6.295505112925526170, 15.36201163567862693, -221.5772643759389098 ) ) ;
#13283 = CARTESIAN_POINT ( 'NONE',  ( 26.54225689383817866, -6.924125931238839016, -230.1506921200174247 ) ) ;
#13284 = DIRECTION ( 'NONE',  ( 0.000000000000000000, 0.000000000000000000, 1.000000000000000000 ) ) ;
#13285 = CARTESIAN_POINT ( 'NONE',  ( -29.22168435891936156, -1.352755938724206519, -225.9547066689444250 ) ) ;
#13286 = CARTESIAN_POINT ( 'NONE',  ( 19.19288224840068935, 10.13059690604263174, -232.1906135022504998 ) ) ;
#13287 = CARTESIAN_POINT ( 'NONE',  ( -3.878264816061211651, -12.95777722686681344, -227.3767537598947683 ) ) ;
#13288 = CARTESIAN_POINT ( 'NONE',  ( 19.02965008953349368, 2.769875716686356348, -226.1578396924859078 ) ) ;
#13289 = CARTESIAN_POINT ( 'NONE',  ( -10.84440549681320221, 27.00404139634608214, -224.0969657459751261 ) ) ;
#13290 = PRESENTATION_STYLE_ASSIGNMENT (( #7681 ) ) ;
#13291 = CARTESIAN_POINT ( 'NONE',  ( 13.20312407767240614, -7.650902547765872086, -230.0578600405493717 ) ) ;
#13292 = CARTESIAN_POINT ( 'NONE',  ( 15.74259730902452858, 17.40808440793174583, -232.1327802909178786 ) ) ;
#13293 = CARTESIAN_POINT ( 'NONE',  ( -4.067324790461362305, 15.10342260507846746, -228.2464404076259257 ) ) ;
#13294 = CARTESIAN_POINT ( 'NONE',  ( -7.099035520468861549, 19.73710792467281649, -233.8745459908100770 ) ) ;
#13295 = ORIENTED_EDGE ( 'NONE', *, *, #11879, .F. ) ;
#13296 = CARTESIAN_POINT ( 'NONE',  ( -26.25663555152313222, -8.728475094464092976, -226.4697227271102236 ) ) ;
#13297 = CARTESIAN_POINT ( 'NONE',  ( 20.64287812348744566, 0.2024751443801864337, -216.7518974727033481 ) ) ;
#13298 = DIRECTION ( 'NONE',  ( 0.000000000000000000, 0.000000000000000000, 1.000000000000000000 ) ) ;
#13299 = CARTESIAN_POINT ( 'NONE',  ( -25.32359575169976296, -0.6821277435459325300, -233.2512658769913969 ) ) ;
#13300 = CARTESIAN_POINT ( 'NONE',  ( 6.771176146757415637, 15.60014285904435027, -218.3493856697694753 ) ) ;
#13301 = CARTESIAN_POINT ( 'NONE',  ( -17.00819119081011266, 8.904695857470725784, -219.7915043529501133 ) ) ;
#13302 = CARTESIAN_POINT ( 'NONE',  ( 10.86206282953156510, 30.27427353967719981, -226.0953027964478110 ) ) ;
#13303 = CARTESIAN_POINT ( 'NONE',  ( 27.79670308438203108, 10.67628923451848877, -225.2981230784098727 ) ) ;
#13304 = CARTESIAN_POINT ( 'NONE',  ( -2.927465716848487887, -13.57531311500885352, -224.4053031992201852 ) ) ;
#13305 = VERTEX_POINT ( 'NONE', #5692 ) ;
#13306 = CARTESIAN_POINT ( 'NONE',  ( -13.53581065110708970, -26.13331550560631555, -224.9773145811678887 ) ) ;
#13307 = CARTESIAN_POINT ( 'NONE',  ( -13.56011990957801139, -0.3895158544032599202, -219.3211261236655218 ) ) ;
#13308 = CARTESIAN_POINT ( 'NONE',  ( 13.99926435381047618, -21.11851526759364006, -232.9234173943665951 ) ) ;
#13309 = CARTESIAN_POINT ( 'NONE',  ( 29.83024462204712179, 0.7507192471929857724, -227.4186229137179396 ) ) ;
#13310 = CARTESIAN_POINT ( 'NONE',  ( -15.22366728182010043, -5.552021002219007961, -230.2511309519622671 ) ) ;
#13311 = CARTESIAN_POINT ( 'NONE',  ( 18.75523091462765990, 19.46592657336209697, -230.4909883316157391 ) ) ;
#13312 = EDGE_CURVE ( 'NONE', #12137, #3391, #19529, .T. ) ;
#13313 = DIRECTION ( 'NONE',  ( 1.000000000000000000, 0.000000000000000000, 0.000000000000000000 ) ) ;
#13314 = CARTESIAN_POINT ( 'NONE',  ( -8.137644474477026435, 12.10064032984799098, -226.6735072060122036 ) ) ;
#13315 = CARTESIAN_POINT ( 'NONE',  ( 8.812670488384366507, 12.21486833790445914, -225.9961634525829197 ) ) ;
#13316 = CARTESIAN_POINT ( 'NONE',  ( -3.082945806077231676, 30.69897765966285874, -224.2387254578930822 ) ) ;
#13317 = CARTESIAN_POINT ( 'NONE',  ( 7.067550969709256670, 17.75197616922148569, -219.3387126207321955 ) ) ;
#13318 = CARTESIAN_POINT ( 'NONE',  ( 14.59690920037431638, -12.12875852167710988, -234.7370354398910877 ) ) ;
#13319 = CARTESIAN_POINT ( 'NONE',  ( -11.07173923371951574, 9.938770595667456575, -229.9381419817434562 ) ) ;
#13320 = CARTESIAN_POINT ( 'NONE',  ( -0.1452471002967452851, 24.29564289358754081, -234.0861481044164805 ) ) ;
#13321 = CARTESIAN_POINT ( 'NONE',  ( -11.82217545354207644, -11.78227988727524966, -219.0934395369134506 ) ) ;
#13322 = CARTESIAN_POINT ( 'NONE',  ( -14.68037037322036475, 3.441677802729143920, -220.1396515630443389 ) ) ;
#13323 = DIRECTION ( 'NONE',  ( 1.000000000000000000, 6.982962677686266711E-15, 0.000000000000000000 ) ) ;
#13324 = CARTESIAN_POINT ( 'NONE',  ( 14.63113973005795643, 4.926264598692385199, -222.4866305912601945 ) ) ;
#13325 = CARTESIAN_POINT ( 'NONE',  ( 12.33825063215758888, -15.78239559842968909, -231.3245247598261471 ) ) ;
#13326 = CARTESIAN_POINT ( 'NONE',  ( -17.49393085256189906, 10.63366922396483361, -217.7502683347138657 ) ) ;
#13327 = CARTESIAN_POINT ( 'NONE',  ( 2.785859284650920031, 14.19821255961969619, -226.9946081512528906 ) ) ;
#13328 = CARTESIAN_POINT ( 'NONE',  ( -23.54665576872953636, -14.78900941482413067, -230.7594827126482073 ) ) ;
#13329 = ITEM_DEFINED_TRANSFORMATION ( 'NONE', 'NONE', #9948,  #6677 ) ;
#13330 = CARTESIAN_POINT ( 'NONE',  ( 16.21758812354607215, 4.665393561625732488, -232.5634757513959983 ) ) ;
#13331 = CARTESIAN_POINT ( 'NONE',  ( 9.253342549662157523, 15.33540844142859605, -216.2601104504267937 ) ) ;
#13332 = ORIENTED_EDGE ( 'NONE', *, *, #15276, .T. ) ;
#13333 = CARTESIAN_POINT ( 'NONE',  ( 5.017623471397871349, 29.83561274492976878, -222.9769172135417250 ) ) ;
#13334 = CARTESIAN_POINT ( 'NONE',  ( 16.69326964758149856, -4.763004462669847783, -219.2590076381798951 ) ) ;
#13335 = CARTESIAN_POINT ( 'NONE',  ( -23.33508647570782557, -8.974881619392299115, 4.459489333929378851 ) ) ;
#13336 = DIRECTION ( 'NONE',  ( -0.000000000000000000, -0.000000000000000000, -1.000000000000000000 ) ) ;
#13337 = CARTESIAN_POINT ( 'NONE',  ( 4.730976410881341465, 17.65764351829336931, -217.6025626048331674 ) ) ;
#13338 = CARTESIAN_POINT ( 'NONE',  ( -4.051702682916754839, -14.52120462818199798, -217.8402208339018671 ) ) ;
#13339 = CARTESIAN_POINT ( 'NONE',  ( 1.729916699924999746, -18.64927252049523432, -233.5000329212076906 ) ) ;
#13340 = CARTESIAN_POINT ( 'NONE',  ( 17.95694455891925756, -3.510678534943489026, -231.2643001502910067 ) ) ;
#13341 = CARTESIAN_POINT ( 'NONE',  ( -12.89119823113977503, 10.10140484475961564, -218.5945808114896636 ) ) ;
#13342 = CARTESIAN_POINT ( 'NONE',  ( 10.79895562092076844, 12.01490073542734116, -225.7380208924852809 ) ) ;
#13343 = DIRECTION ( 'NONE',  ( -0.000000000000000000, -0.000000000000000000, -1.000000000000000000 ) ) ;
#13344 = CARTESIAN_POINT ( 'NONE',  ( -21.95649697515285581, 20.70968357470995258, -226.9638023349746447 ) ) ;
#13345 = CARTESIAN_POINT ( 'NONE',  ( -15.02851318684991000, -5.270497739200964205, -221.5518599052197146 ) ) ;
#13346 = ORIENTED_EDGE ( 'NONE', *, *, #19894, .T. ) ;
#13347 = CARTESIAN_POINT ( 'NONE',  ( -10.23029362138610843, 26.44342627367518617, -221.6879936327511871 ) ) ;
#13348 = CARTESIAN_POINT ( 'NONE',  ( 27.79746884017060538, 13.63637251724950339, -226.5788410723774575 ) ) ;
#13349 = CARTESIAN_POINT ( 'NONE',  ( 8.036750260989780514, 26.29729070384984624, -233.5018314387838529 ) ) ;
#13350 = CARTESIAN_POINT ( 'NONE',  ( 12.90505172109588194, -11.18139282378177768, -218.7382941517081747 ) ) ;
#13351 = CARTESIAN_POINT ( 'NONE',  ( 0.000000000000000000, 0.000000000000000000, 94.00000000000000000 ) ) ;
#13352 = EDGE_LOOP ( 'NONE', ( #6366, #7049, #21430, #11007 ) ) ;
#13353 = CARTESIAN_POINT ( 'NONE',  ( -15.48255455842386219, 10.01793346089237069, -233.1197357361336913 ) ) ;
#13354 = CARTESIAN_POINT ( 'NONE',  ( -11.58651333402397476, -12.19597367159924595, -216.5418320517508448 ) ) ;
#13355 = CARTESIAN_POINT ( 'NONE',  ( 12.23063869552301242, 12.84118223717021934, -218.8273164334868284 ) ) ;
#13356 = DIRECTION ( 'NONE',  ( 0.000000000000000000, 0.000000000000000000, -1.000000000000000000 ) ) ;
#13357 = CARTESIAN_POINT ( 'NONE',  ( 8.785770181087007913, -10.38731345016515917, -223.4272116603623317 ) ) ;
#13358 = CARTESIAN_POINT ( 'NONE',  ( -24.68906941503829700, 2.445024713909649705, -232.6803430500543755 ) ) ;
#13359 = PRODUCT_DEFINITION_SHAPE ( 'NONE', 'NONE',  #22270 ) ;
#13360 = CARTESIAN_POINT ( 'NONE',  ( -18.70090456008720992, 23.36146401084868884, -220.3989740370807056 ) ) ;
#13361 = EDGE_CURVE ( 'NONE', #21305, #5604, #18535, .T. ) ;
#13362 = CARTESIAN_POINT ( 'NONE',  ( 22.42095341476093040, 9.457779162868732215, -232.6339572190428555 ) ) ;
#13363 = SURFACE_SIDE_STYLE ('',( #9660 ) ) ;
#13364 = AXIS2_PLACEMENT_3D ( 'NONE', #17956, #836, #2631 ) ;
#13365 = CARTESIAN_POINT ( 'NONE',  ( -3.400000000000003908, 0.000000000000000000, -224.9999999999999716 ) ) ;
#13366 = CARTESIAN_POINT ( 'NONE',  ( 15.01439307471096463, 1.118969480519667048, -226.7488225241675366 ) ) ;
#13367 = DIRECTION ( 'NONE',  ( 1.000000000000000000, 0.000000000000000000, 0.000000000000000000 ) ) ;
#13368 = CARTESIAN_POINT ( 'NONE',  ( 14.80019294276752007, -6.608272808847591051, -224.1005182637183566 ) ) ;
#13369 = CARTESIAN_POINT ( 'NONE',  ( -26.43144772945995413, -6.745116643720071359, -219.5134289301136050 ) ) ;
#13370 = DIRECTION ( 'NONE',  ( 0.000000000000000000, 0.000000000000000000, -1.000000000000000000 ) ) ;
#13371 = CIRCLE ( 'NONE', #9773, 23.00000000000000000 ) ;
#13372 = CARTESIAN_POINT ( 'NONE',  ( 0.000000000000000000, 0.000000000000000000, 75.00000000000000000 ) ) ;
#13373 = CARTESIAN_POINT ( 'NONE',  ( 5.711092584709906106, 26.13380667269736790, -220.5232813324456629 ) ) ;
#13374 = CARTESIAN_POINT ( 'NONE',  ( 10.74287257054252720, -16.14773823008032849, -215.8883494958819824 ) ) ;
#13375 = CARTESIAN_POINT ( 'NONE',  ( 21.39922646226391478, -21.53954253117021977, -224.1701659532164967 ) ) ;
#13376 = CARTESIAN_POINT ( 'NONE',  ( -14.87932799058895128, 18.71706570923887369, -231.8731726670167745 ) ) ;
#13377 = CARTESIAN_POINT ( 'NONE',  ( 12.88374853655145458, 4.106359831454843068, -228.1016120772327440 ) ) ;
#13378 = CARTESIAN_POINT ( 'NONE',  ( 12.56556766396551872, 9.776144415819011613, -223.4791766911294815 ) ) ;
#13379 = EDGE_LOOP ( 'NONE', ( #20473, #18561, #6712, #17203 ) ) ;
#13380 = CARTESIAN_POINT ( 'NONE',  ( -8.507271545618831254, -16.45592803179997787, -230.0780227380557790 ) ) ;
#13381 = CARTESIAN_POINT ( 'NONE',  ( 0.000000000000000000, -23.00000000000006040, -24.99999999999999645 ) ) ;
#13382 = CARTESIAN_POINT ( 'NONE',  ( -12.13692969104051400, -0.3108940857385004697, -222.6170402347994184 ) ) ;
#13383 = CARTESIAN_POINT ( 'NONE',  ( 14.28815361401014172, 13.86049093364188778, -216.0585456615740156 ) ) ;
#13384 = CARTESIAN_POINT ( 'NONE',  ( 27.38348740615853316, -3.050674415727137045, -231.0934891209028876 ) ) ;
#13385 = CARTESIAN_POINT ( 'NONE',  ( 4.907833106823921376, 13.98151846258800290, -229.0190609869640923 ) ) ;
#13386 = CARTESIAN_POINT ( 'NONE',  ( -12.31207293045244988, 6.732038552366256923, -221.0952066824360713 ) ) ;
#13387 = VECTOR ( 'NONE', #4948, 1000.000000000000000 ) ;
#13388 = CARTESIAN_POINT ( 'NONE',  ( 9.616550234602936342, 9.263684773868845923, -230.4827401731016607 ) ) ;
#13389 = EDGE_CURVE ( 'NONE', #4564, #645, #11297, .T. ) ;
#13390 = CARTESIAN_POINT ( 'NONE',  ( -17.91769793922991028, 3.277678596821882007, -219.5526088240203819 ) ) ;
#13391 = CARTESIAN_POINT ( 'NONE',  ( -17.75316132689678383, 25.03468689048078843, -222.1645193425721061 ) ) ;
#13392 = CARTESIAN_POINT ( 'NONE',  ( -7.387516090585421580, 7.838405800256096789, 92.00000000000001421 ) ) ;
#13393 = CARTESIAN_POINT ( 'NONE',  ( 14.02816775221371337, 20.58276248714641810, -218.7180790146936999 ) ) ;
#13394 = DIRECTION ( 'NONE',  ( 0.000000000000000000, 0.000000000000000000, -1.000000000000000000 ) ) ;
#13395 = CARTESIAN_POINT ( 'NONE',  ( -22.05223281125446633, 0.4748437386657422543, -217.8785187290425256 ) ) ;
#13396 = CARTESIAN_POINT ( 'NONE',  ( -14.70339349403010942, -0.4153334646997780544, -217.8790668391084466 ) ) ;
#13397 = CARTESIAN_POINT ( 'NONE',  ( -13.13215111221786024, -8.938624195428067409, -226.3235457059856515 ) ) ;
#13398 = VECTOR ( 'NONE', #12530, 1000.000000000000000 ) ;
#13399 = CARTESIAN_POINT ( 'NONE',  ( -3.000000000000034195, -6.000000000000006217, -227.9999999999999716 ) ) ;
#13400 = CIRCLE ( 'NONE', #5494, 21.63401512838757768 ) ;
#13401 = CARTESIAN_POINT ( 'NONE',  ( -4.130417896617784912, 16.21758012034559826, -229.8171973319304584 ) ) ;
#13402 = CARTESIAN_POINT ( 'NONE',  ( 2.936803900436826709, -18.74190719154852758, -218.5197582523356061 ) ) ;
#13403 = EDGE_CURVE ( 'NONE', #12667, #21337, #21341, .T. ) ;
#13404 = CARTESIAN_POINT ( 'NONE',  ( 12.55473222622303986, 11.30320364856893001, -218.8964119182764989 ) ) ;
#13405 = CARTESIAN_POINT ( 'NONE',  ( -4.691002462566371101, 21.98518063340150164, -232.2516024630330094 ) ) ;
#13406 = CARTESIAN_POINT ( 'NONE',  ( -10.14083745617744547, 19.87482866967577877, -216.0596634563153486 ) ) ;
#13407 = VERTEX_POINT ( 'NONE', #851 ) ;
#13408 = CARTESIAN_POINT ( 'NONE',  ( -18.57671526409105667, -15.84599122335686161, -218.9973662248357300 ) ) ;
#13409 = CARTESIAN_POINT ( 'NONE',  ( 11.13678936984666912, 26.95732789089726111, -228.8350761760834757 ) ) ;
#13410 = ADVANCED_FACE ( 'NONE', ( #18189, #4000 ), #10994, .F. ) ;
#13411 = CARTESIAN_POINT ( 'NONE',  ( 17.96045420455031305, -0.3746358454349600908, -217.9627609769914613 ) ) ;
#13412 = ADVANCED_FACE ( 'NONE', ( #21434 ), #4093, .T. ) ;
#13413 = DIRECTION ( 'NONE',  ( -1.000000000000000000, 0.000000000000000000, 0.000000000000000000 ) ) ;
#13414 = CARTESIAN_POINT ( 'NONE',  ( 24.21331552874348958, 0.07051084380047288602, -231.7986140076958463 ) ) ;
#13415 = CARTESIAN_POINT ( 'NONE',  ( 12.74913679152205148, 9.185760885856177893, -218.6542381594888980 ) ) ;
#13416 = CIRCLE ( 'NONE', #6586, 23.00000000000008882 ) ;
#13417 = CARTESIAN_POINT ( 'NONE',  ( -21.99356461413155728, 5.827088221545293045, -219.1725956997024127 ) ) ;
#13418 = VECTOR ( 'NONE', #11901, 1000.000000000000000 ) ;
#13419 = CARTESIAN_POINT ( 'NONE',  ( -2.328291070394212792, 14.80737693666302945, -219.0291440940735868 ) ) ;
#13420 = CARTESIAN_POINT ( 'NONE',  ( 14.92135368508905202, 7.451356898669101447, -219.1823315336843621 ) ) ;
#13421 = ORIENTED_EDGE ( 'NONE', *, *, #2389, .F. ) ;
#13422 = CARTESIAN_POINT ( 'NONE',  ( -6.651864601267788224, -12.12497212411570580, -228.9083653044881714 ) ) ;
#13423 = VERTEX_POINT ( 'NONE', #9309 ) ;
#13424 = CARTESIAN_POINT ( 'NONE',  ( -14.34029329777712469, -14.57793623142476669, -217.2545494607695389 ) ) ;
#13425 = CARTESIAN_POINT ( 'NONE',  ( -22.04004491965229207, 12.41871177236473578, -215.2165492276571115 ) ) ;
#13426 = CARTESIAN_POINT ( 'NONE',  ( 7.080148886126969465, -28.65852557119563926, -219.9679292432588227 ) ) ;
#13427 = CARTESIAN_POINT ( 'NONE',  ( 21.26068545928058384, -3.181857413669367141, -233.8217025890263585 ) ) ;
#13428 = CARTESIAN_POINT ( 'NONE',  ( -24.76115377241536208, -2.015397159694146456, -231.8500816169410825 ) ) ;
#13429 = CARTESIAN_POINT ( 'NONE',  ( 8.812670488384366507, 12.21486833790445914, -225.9961634525829197 ) ) ;
#13430 = SURFACE_STYLE_USAGE ( .BOTH. , #11854 ) ;
#13431 = CARTESIAN_POINT ( 'NONE',  ( -14.60180519431160917, 24.46340507526420893, -221.8423643191928534 ) ) ;
#13432 = CARTESIAN_POINT ( 'NONE',  ( 10.14297843322460402, 14.69845403004500639, -219.2805000163441207 ) ) ;
#13433 = CARTESIAN_POINT ( 'NONE',  ( 22.46220731426537043, 18.23201731183003460, -227.5436199598787539 ) ) ;
#13434 = CARTESIAN_POINT ( 'NONE',  ( 15.03112630398312177, 24.11065413595933293, -226.8236212149936080 ) ) ;
#13435 = CARTESIAN_POINT ( 'NONE',  ( 17.14704237169575052, -19.77033640698606121, -215.4809218419665342 ) ) ;
#13436 = AXIS2_PLACEMENT_3D ( 'NONE', #12261, #3691, #10575 ) ;
#13437 = CIRCLE ( 'NONE', #8777, 20.99999999999999645 ) ;
#13438 = CARTESIAN_POINT ( 'NONE',  ( -2.328291070394212792, 14.80737693666302945, -219.0291440940735868 ) ) ;
#13439 = CYLINDRICAL_SURFACE ( 'NONE', #10838, 17.50000000000000711 ) ;
#13440 = DIRECTION ( 'NONE',  ( -1.000000000000000000, 0.000000000000000000, 2.891205793294678696E-17 ) ) ;
#13441 = CARTESIAN_POINT ( 'NONE',  ( 10.57926812561479757, 10.00910231482511215, -225.8341706491384286 ) ) ;
#13442 = CARTESIAN_POINT ( 'NONE',  ( 8.222674095483935020, -17.25680718911290512, -231.8150392270642612 ) ) ;
#13443 = CARTESIAN_POINT ( 'NONE',  ( -22.07068341299880743, 18.38202870573248049, -227.7785760498121306 ) ) ;
#13444 = CARTESIAN_POINT ( 'NONE',  ( -4.855966894080006035, 26.75753167227873064, -230.1547293463117114 ) ) ;
#13445 = CARTESIAN_POINT ( 'NONE',  ( -16.05483997570105714, -7.226811045751038165, -218.5819178105544438 ) ) ;
#13446 = CARTESIAN_POINT ( 'NONE',  ( -26.64664107080812627, 5.256684826493772000, -228.0533579629717735 ) ) ;
#13447 = PRODUCT_RELATED_PRODUCT_CATEGORY ( 'part', '', ( #10326 ) ) ;
#13448 = CARTESIAN_POINT ( 'NONE',  ( 8.343316395906509086, 11.57404413652245800, -231.1403332574589911 ) ) ;
#13449 = CARTESIAN_POINT ( 'NONE',  ( 5.169766346882679997, 29.28517558595074988, -221.5178724947562614 ) ) ;
#13450 = CARTESIAN_POINT ( 'NONE',  ( 12.14783608763084644, -10.95966212275308571, -222.8518398773795184 ) ) ;
#13451 = CARTESIAN_POINT ( 'NONE',  ( 23.27685575300125720, -16.81362096763192326, -220.1650456318757563 ) ) ;
#13452 = DIRECTION ( 'NONE',  ( -0.000000000000000000, -0.000000000000000000, -1.000000000000000000 ) ) ;
#13453 = CIRCLE ( 'NONE', #13822, 19.80000000000007887 ) ;
#13454 = CARTESIAN_POINT ( 'NONE',  ( 7.168644370073567806, 19.32044210858112265, -233.1278450877711634 ) ) ;
#13455 = CARTESIAN_POINT ( 'NONE',  ( -12.17842630902860712, -4.030040138803427929, -228.6515579410213661 ) ) ;
#13456 = CARTESIAN_POINT ( 'NONE',  ( -5.525229149912007642, -13.32411127922494742, -220.4018445532201440 ) ) ;
#13457 = CARTESIAN_POINT ( 'NONE',  ( 13.91151814069282722, -15.58123622716646572, -216.5183035683795367 ) ) ;
#13458 = CARTESIAN_POINT ( 'NONE',  ( -27.40681729237160269, 15.04232492504307572, -225.3323746796125704 ) ) ;
#13459 = CARTESIAN_POINT ( 'NONE',  ( 9.322595869360968734, 23.38184458253662967, -230.2763482547081821 ) ) ;
#13460 = CARTESIAN_POINT ( 'NONE',  ( -22.11084984981285118, 10.96048252433489623, -216.6117774006995376 ) ) ;
#13461 = CARTESIAN_POINT ( 'NONE',  ( -31.04267853410473421, 7.029517189377418873, -226.8060334161593516 ) ) ;
#13462 = CARTESIAN_POINT ( 'NONE',  ( -15.65746202990257174, -5.535581341804817868, -220.4933418326074559 ) ) ;
#13463 = ORIENTED_EDGE ( 'NONE', *, *, #4223, .T. ) ;
#13464 = CARTESIAN_POINT ( 'NONE',  ( -7.250603130619442283, 20.89725557392719324, -217.7893896917081520 ) ) ;
#13465 = CARTESIAN_POINT ( 'NONE',  ( 12.96449997971774870, 8.285709878278680662, -230.9518598506670628 ) ) ;
#13466 = CARTESIAN_POINT ( 'NONE',  ( -5.974114889119001681, 17.52937113675171332, -232.3862906442651592 ) ) ;
#13467 = CARTESIAN_POINT ( 'NONE',  ( 14.49023023880111083, -12.14520762395643061, -217.6171285705176501 ) ) ;
#13468 = DIRECTION ( 'NONE',  ( -0.000000000000000000, -0.000000000000000000, -1.000000000000000000 ) ) ;
#13469 = ORIENTED_EDGE ( 'NONE', *, *, #19326, .F. ) ;
#13470 = CARTESIAN_POINT ( 'NONE',  ( -12.74846050492543625, 19.93509882904884734, -216.0172840992881049 ) ) ;
#13471 = CARTESIAN_POINT ( 'NONE',  ( -30.53557093151922430, -9.496448454471346778, -222.0905184547210638 ) ) ;
#13472 = CARTESIAN_POINT ( 'NONE',  ( 1.322875655532295358, 1.500000000000000000, -378.2244600276337678 ) ) ;
#13473 = TOROIDAL_SURFACE ( 'NONE', #19217, 22.56777165119825668, 5.000000000000000000 ) ;
#13474 = CARTESIAN_POINT ( 'NONE',  ( 5.623554730548537606, 15.65270319720736225, -231.3185741195121068 ) ) ;
#13475 = DIRECTION ( 'NONE',  ( -1.000000000000000000, 0.000000000000000000, 0.000000000000000000 ) ) ;
#13476 =( GEOMETRIC_REPRESENTATION_CONTEXT ( 3 ) GLOBAL_UNCERTAINTY_ASSIGNED_CONTEXT ( ( #21344 ) ) GLOBAL_UNIT_ASSIGNED_CONTEXT ( ( #11346, #6493, #21905 ) ) REPRESENTATION_CONTEXT ( 'NONE', 'WORKASPACE' ) );
#13477 = CARTESIAN_POINT ( 'NONE',  ( 20.98776729843937972, -13.55153944770713359, -217.5092423276211946 ) ) ;
#13478 = CARTESIAN_POINT ( 'NONE',  ( -29.30406754532526037, 5.063969254119831120, -221.8212091093853076 ) ) ;
#13479 = CARTESIAN_POINT ( 'NONE',  ( -13.43384090552117271, 6.057765724406720231, -225.7182623230366119 ) ) ;
#13480 = CARTESIAN_POINT ( 'NONE',  ( 18.79638869589749461, 0.4878066561304963966, -219.5712168927955759 ) ) ;
#13481 = CARTESIAN_POINT ( 'NONE',  ( -10.03082531488024109, -22.09229706162428286, -231.9736132431984572 ) ) ;
#13482 = DIRECTION ( 'NONE',  ( 0.000000000000000000, 0.000000000000000000, 1.000000000000000000 ) ) ;
#13483 = CARTESIAN_POINT ( 'NONE',  ( 27.40550551777678123, 5.967061366481472895, -228.7463788799179554 ) ) ;
#13484 = CARTESIAN_POINT ( 'NONE',  ( 0.000000000000000000, 0.000000000000000000, -69.99999999999998579 ) ) ;
#13485 = CARTESIAN_POINT ( 'NONE',  ( 20.53618124091710939, -19.36892006637360097, -226.5121684596580849 ) ) ;
#13486 = CARTESIAN_POINT ( 'NONE',  ( 13.10740018641116400, -2.248054146740232184, -226.9883072097889567 ) ) ;
#13487 = EDGE_CURVE ( 'NONE', #9939, #14043, #14889, .T. ) ;
#13488 = CARTESIAN_POINT ( 'NONE',  ( -20.71220452560666203, -10.00022918515372794, 0.3239426289883403642 ) ) ;
#13489 = CARTESIAN_POINT ( 'NONE',  ( 2.601379523478754674, 17.36677895276155681, -230.4357129074444117 ) ) ;
#13490 = CARTESIAN_POINT ( 'NONE',  ( 6.114261689233397412, -11.26162238963769369, -223.0577857700231164 ) ) ;
#13491 = AXIS2_PLACEMENT_3D ( 'NONE', #20914, #10465, #10695 ) ;
#13492 = CARTESIAN_POINT ( 'NONE',  ( 15.11994912051959972, -12.48385213956034079, -232.8079920308188377 ) ) ;
#13493 = EDGE_LOOP ( 'NONE', ( #13224, #15607, #5510, #21117 ) ) ;
#13494 = AXIS2_PLACEMENT_3D ( 'NONE', #1384, #20495, #17250 ) ;
#13495 = CARTESIAN_POINT ( 'NONE',  ( -15.11329978779464689, 11.41628732213579411, -231.7124318929555500 ) ) ;
#13496 = CARTESIAN_POINT ( 'NONE',  ( 15.91624278015930649, 5.932232821383347954, -217.3600859879243217 ) ) ;
#13497 = CARTESIAN_POINT ( 'NONE',  ( 13.71585692689473213, 6.523039003617190801, -224.4540437369149402 ) ) ;
#13498 = ORIENTED_EDGE ( 'NONE', *, *, #4247, .T. ) ;
#13499 = CARTESIAN_POINT ( 'NONE',  ( -8.398697845537501649, -22.62202615048447640, -219.0766901614751703 ) ) ;
#13500 = DIRECTION ( 'NONE',  ( 0.000000000000000000, 0.000000000000000000, 1.000000000000000000 ) ) ;
#13501 = CARTESIAN_POINT ( 'NONE',  ( -13.56011990957801139, -0.3895158544032599202, -219.3211261236655218 ) ) ;
#13502 = ORIENTED_EDGE ( 'NONE', *, *, #16439, .T. ) ;
#13503 = CARTESIAN_POINT ( 'NONE',  ( 4.914880347045685660, 14.54749271951947698, -232.8668677254037789 ) ) ;
#13504 = CARTESIAN_POINT ( 'NONE',  ( 10.07328213880649592, -15.27579949576245966, -229.4560222226588451 ) ) ;
#13505 = CARTESIAN_POINT ( 'NONE',  ( 8.689059922489732912, 15.18271246186214363, -218.7354841152034908 ) ) ;
#13506 = CARTESIAN_POINT ( 'NONE',  ( -26.74045434827795020, 12.41518252455047744, -220.4617428697642652 ) ) ;
#13507 = CARTESIAN_POINT ( 'NONE',  ( 3.711349367426693746, 16.84755988915346236, -233.7359972593521888 ) ) ;
#13508 = CIRCLE ( 'NONE', #19596, 21.63401512838748175 ) ;
#13509 = CARTESIAN_POINT ( 'NONE',  ( -26.70018640714903668, 3.110792036746048428, -228.8761207540193823 ) ) ;
#13510 = CARTESIAN_POINT ( 'NONE',  ( -2.735889804569492600, 12.71735652435744512, -225.1194195722198117 ) ) ;
#13511 = CARTESIAN_POINT ( 'NONE',  ( 14.80394259695730064, 1.224172658189580432, -225.4564070658925061 ) ) ;
#13512 = CARTESIAN_POINT ( 'NONE',  ( -1.643553855084622928, -13.05119293000219294, -222.7191902239112551 ) ) ;
#13513 = CARTESIAN_POINT ( 'NONE',  ( 23.12216041205843453, 0.2121350054995089496, -232.0572713672589202 ) ) ;
#13514 = CARTESIAN_POINT ( 'NONE',  ( 1.665334536937735820E-13, -23.00000000000006040, -69.99999999999998579 ) ) ;
#13515 = CARTESIAN_POINT ( 'NONE',  ( -21.80830016239255897, -4.781675611938959847, -217.4666014280278148 ) ) ;
#13516 = CARTESIAN_POINT ( 'NONE',  ( -20.73319232323294514, 5.144688277016327582, -214.6391322078443977 ) ) ;
#13517 = CARTESIAN_POINT ( 'NONE',  ( -14.92584319327083442, -9.764953932613968490, -229.6443584147421006 ) ) ;
#13518 = CARTESIAN_POINT ( 'NONE',  ( 0.000000000000000000, 0.000000000000000000, 80.43141006107198621 ) ) ;
#13519 = CARTESIAN_POINT ( 'NONE',  ( 10.46316887740464985, -17.92901728017801233, -232.6108895528913081 ) ) ;
#13520 = CARTESIAN_POINT ( 'NONE',  ( 20.40268796714816801, 18.65534563792085621, -219.5587498978784993 ) ) ;
#13521 = CARTESIAN_POINT ( 'NONE',  ( -10.40174557315337900, 22.75579539577861965, -231.4492192189165962 ) ) ;
#13522 = CARTESIAN_POINT ( 'NONE',  ( -14.84124724799726991, 21.42277200659090042, -233.6300684249849553 ) ) ;
#13523 = ORIENTED_EDGE ( 'NONE', *, *, #598, .T. ) ;
#13524 = CARTESIAN_POINT ( 'NONE',  ( 13.95860357795928941, -2.197645239214564672, -231.3209047126647988 ) ) ;
#13525 = ORIENTED_EDGE ( 'NONE', *, *, #14266, .T. ) ;
#13526 = AXIS2_PLACEMENT_3D ( 'NONE', #15563, #2048, #5531 ) ;
#13527 = CARTESIAN_POINT ( 'NONE',  ( 6.093530912645064745, 16.79941505724243811, -232.1766444656230419 ) ) ;
#13528 = EDGE_CURVE ( 'NONE', #11, #21087, #740, .T. ) ;
#13529 = CIRCLE ( 'NONE', #8857, 3.000000000000002665 ) ;
#13530 = CARTESIAN_POINT ( 'NONE',  ( -21.89065952084834166, -0.9940043559354216907, -218.9999999999999716 ) ) ;
#13531 = CARTESIAN_POINT ( 'NONE',  ( 25.70350299105564318, 4.008313962570879241, -233.1578316763087173 ) ) ;
#13532 = CARTESIAN_POINT ( 'NONE',  ( 1.665334536937735820E-13, -23.00000000000006040, 69.99999999999998579 ) ) ;
#13533 = CARTESIAN_POINT ( 'NONE',  ( -15.95680269303277221, -1.471987722620473615, -218.5035227479738751 ) ) ;
#13534 = PRODUCT_DEFINITION_FORMATION_WITH_SPECIFIED_SOURCE ( 'ANY', '', #16780, .NOT_KNOWN. ) ;
#13535 = CARTESIAN_POINT ( 'NONE',  ( 23.22505041959077232, 19.39625294115234055, -221.5972645870541555 ) ) ;
#13536 = CARTESIAN_POINT ( 'NONE',  ( -23.67953786836281083, 9.946055673977088674, -229.5560005648173671 ) ) ;
#13537 = CARTESIAN_POINT ( 'NONE',  ( 1.984991703947643904, 14.51738422979996912, -218.4500278854917781 ) ) ;
#13538 = ADVANCED_FACE ( 'NONE', ( #4325, #11648 ), #9741, .T. ) ;
#13539 = CARTESIAN_POINT ( 'NONE',  ( 16.77055746703809191, 7.081497542956901370, -232.0295235404293521 ) ) ;
#13540 = AXIS2_PLACEMENT_3D ( 'NONE', #4614, #18356, #16784 ) ;
#13541 = CARTESIAN_POINT ( 'NONE',  ( -9.654146510541638193, -9.431978497097317060, -229.7352898675592314 ) ) ;
#13542 = ORIENTED_EDGE ( 'NONE', *, *, #16056, .F. ) ;
#13543 = CARTESIAN_POINT ( 'NONE',  ( -18.38002254392888446, -21.81807606669838506, -229.0374583293157968 ) ) ;
#13544 = CARTESIAN_POINT ( 'NONE',  ( -26.42613204384124259, 13.88327151024443395, -218.2510073314678323 ) ) ;
#13545 = CARTESIAN_POINT ( 'NONE',  ( 15.34510829589250491, -24.56813251781886009, -230.1307231235174982 ) ) ;
#13546 = CARTESIAN_POINT ( 'NONE',  ( -0.1571923090946999446, 19.34188126963334398, -216.6893131123363787 ) ) ;
#13547 = CARTESIAN_POINT ( 'NONE',  ( 14.51690190576628048, -4.522004643715366257, -218.3468014590714859 ) ) ;
#13548 = CARTESIAN_POINT ( 'NONE',  ( -24.15031621174628285, -13.05338392360020627, -219.0842748323915714 ) ) ;
#13549 = CARTESIAN_POINT ( 'NONE',  ( 12.55473222622303986, 11.30320364856893001, -218.8964119182764989 ) ) ;
#13550 = PRODUCT_DEFINITION_FORMATION_WITH_SPECIFIED_SOURCE ( 'ANY', '', #10326, .NOT_KNOWN. ) ;
#13551 = CARTESIAN_POINT ( 'NONE',  ( 21.50000000000001066, 2.632990618166810813E-15, -30.00000000000000000 ) ) ;
#13552 = CARTESIAN_POINT ( 'NONE',  ( -10.30040261405712698, 19.75576125044891285, -218.0811964201226658 ) ) ;
#13553 = CARTESIAN_POINT ( 'NONE',  ( 9.125049424194871861, 12.37796447639467523, -227.2539065556229332 ) ) ;
#13554 = CARTESIAN_POINT ( 'NONE',  ( 23.04897566969193079, 17.95862962700741861, -223.6438515760422661 ) ) ;
#13555 = CARTESIAN_POINT ( 'NONE',  ( 9.125049424194871861, 12.37796447639467523, -227.2539065556229332 ) ) ;
#13556 = CARTESIAN_POINT ( 'NONE',  ( 0.5573677079071300833, -14.80782849724859496, -218.9269569601107719 ) ) ;
#13557 = CARTESIAN_POINT ( 'NONE',  ( -9.523248388595575875, 12.31121908620753125, -221.6288572946744182 ) ) ;
#13558 = PRODUCT ( 'Soft-Touch Power _ Function Switch', 'Soft-Touch Power _ Function Switch', '', ( #4546 ) ) ;
#13559 = CARTESIAN_POINT ( 'NONE',  ( 0.000000000000000000, 0.000000000000000000, -25.00000000000000000 ) ) ;
#13560 = CARTESIAN_POINT ( 'NONE',  ( 22.97235139684061878, 0.000000000000000000, 75.01817430661621700 ) ) ;
#13561 = CARTESIAN_POINT ( 'NONE',  ( 24.03642272140365677, 3.646960756862087205, -218.2320643939070806 ) ) ;
#13562 = CARTESIAN_POINT ( 'NONE',  ( 3.692943796146577196, -17.43777048755501724, -232.3481250940208156 ) ) ;
#13563 = CARTESIAN_POINT ( 'NONE',  ( -13.75208518020500748, 5.661250135068270239, -227.6647651141479685 ) ) ;
#13564 = CARTESIAN_POINT ( 'NONE',  ( -0.7041916573665241152, 14.60214745152014437, -226.3818583194645555 ) ) ;
#13565 = CARTESIAN_POINT ( 'NONE',  ( -11.20272313682045073, -7.956653478762055087, -225.3025344850567819 ) ) ;
#13566 = CARTESIAN_POINT ( 'NONE',  ( -20.41147829968989313, 3.432784889297933795, -230.9611049257633510 ) ) ;
#13567 = CARTESIAN_POINT ( 'NONE',  ( 24.81668481317358399, 17.11438712655213124, -222.1096362285750274 ) ) ;
#13568 = ORIENTED_EDGE ( 'NONE', *, *, #8542, .T. ) ;
#13569 = CARTESIAN_POINT ( 'NONE',  ( -9.716674560061926869, 27.56227806819028103, -219.4917914922789919 ) ) ;
#13570 = CARTESIAN_POINT ( 'NONE',  ( 14.06411491198613462, -8.094314315948059502, -222.2253600114596566 ) ) ;
#13571 = CARTESIAN_POINT ( 'NONE',  ( 12.90505172109588194, -11.18139282378177768, -218.7382941517081747 ) ) ;
#13572 = DIRECTION ( 'NONE',  ( 1.000000000000000000, 0.000000000000000000, 0.000000000000000000 ) ) ;
#13573 = CARTESIAN_POINT ( 'NONE',  ( 11.13678936984666912, 26.95732789089726111, -228.8350761760834757 ) ) ;
#13574 = CARTESIAN_POINT ( 'NONE',  ( -9.690988788510356500, -7.266623515821958534, -222.7221403394456445 ) ) ;
#13575 = CARTESIAN_POINT ( 'NONE',  ( -6.052919920376759855, -15.38051382379660836, -218.0337201863237624 ) ) ;
#13576 = CARTESIAN_POINT ( 'NONE',  ( 15.34510829589250491, -24.56813251781886009, -230.1307231235174982 ) ) ;
#13577 = CARTESIAN_POINT ( 'NONE',  ( -18.17591565587962776, 16.23604867791855355, -233.2845329962925121 ) ) ;
#13578 = CARTESIAN_POINT ( 'NONE',  ( 12.84032013659066251, 19.10303921738740485, -230.8110334357214128 ) ) ;
#13579 = CARTESIAN_POINT ( 'NONE',  ( -27.82842955277035202, 11.70195273568964112, -227.9294339757464911 ) ) ;
#13580 = CARTESIAN_POINT ( 'NONE',  ( -25.98311979368102342, 15.13734258059737670, -220.6162231662327429 ) ) ;
#13581 = CARTESIAN_POINT ( 'NONE',  ( -15.57180599510074437, -4.609960555941468918, -228.7341395176208323 ) ) ;
#13582 = EDGE_LOOP ( 'NONE', ( #4218, #14367 ) ) ;
#13583 = CARTESIAN_POINT ( 'NONE',  ( -4.715783688792956063, 28.29821729825949816, -228.0423900005874600 ) ) ;
#13584 = CARTESIAN_POINT ( 'NONE',  ( 29.89309326230132058, 6.052383583152112223, -228.3539431708548477 ) ) ;
#13585 = CARTESIAN_POINT ( 'NONE',  ( 5.264801124131998300, 10.54092478143144795, -226.4890466082630098 ) ) ;
#13586 = CARTESIAN_POINT ( 'NONE',  ( 22.55746627616819566, -14.21542447219996852, -231.9819121152456205 ) ) ;
#13587 = DIRECTION ( 'NONE',  ( 0.000000000000000000, 0.000000000000000000, 1.000000000000000000 ) ) ;
#13588 = VERTEX_POINT ( 'NONE', #2969 ) ;
#13589 = CARTESIAN_POINT ( 'NONE',  ( -6.571166997218196748, 12.74865329367398736, -229.9840124400968762 ) ) ;
#13590 = CARTESIAN_POINT ( 'NONE',  ( -14.38198375515248273, -6.747285987484331393, -233.1569015480179985 ) ) ;
#13591 = LINE ( 'NONE', #11893, #7273 ) ;
#13592 = CARTESIAN_POINT ( 'NONE',  ( 14.95414693437772868, 8.262206471704862665, -230.1862972580043163 ) ) ;
#13593 = CARTESIAN_POINT ( 'NONE',  ( 0.000000000000000000, 0.000000000000000000, -77.51594804401857175 ) ) ;
#13594 = CARTESIAN_POINT ( 'NONE',  ( 14.18709644517307922, -11.45356969546147496, -232.2178450427173004 ) ) ;
#13595 = CARTESIAN_POINT ( 'NONE',  ( -19.25929423112888017, 9.818144317380269825, -216.1837936240308409 ) ) ;
#13596 = EDGE_CURVE ( 'NONE', #21305, #722, #10931, .T. ) ;
#13597 = CARTESIAN_POINT ( 'NONE',  ( 14.92135368508905202, 7.451356898669101447, -219.1823315336843621 ) ) ;
#13598 = CARTESIAN_POINT ( 'NONE',  ( -13.01444359484612079, -23.32256785062423887, -219.1545357706015693 ) ) ;
#13599 = DIRECTION ( 'NONE',  ( -0.000000000000000000, -0.000000000000000000, 1.000000000000000000 ) ) ;
#13600 = CARTESIAN_POINT ( 'NONE',  ( 22.03647168420945590, 0.3315607655625663064, -232.0572713672586644 ) ) ;
#13601 = CARTESIAN_POINT ( 'NONE',  ( -16.71711190488355570, 0.6105529133557690002, -230.9511258789794681 ) ) ;
#13602 = CARTESIAN_POINT ( 'NONE',  ( 12.33825063215758888, -15.78239559842968909, -231.3245247598261471 ) ) ;
#13603 = CARTESIAN_POINT ( 'NONE',  ( -29.27492217116574480, -1.185422171198730501, -224.8132346143397342 ) ) ;
#13604 = CARTESIAN_POINT ( 'NONE',  ( 22.00000000000000000, 6.162975822039154730E-30, -228.0000000000000000 ) ) ;
#13605 = CARTESIAN_POINT ( 'NONE',  ( 12.00334754111224100, 12.62951371569041115, -228.5814949098771649 ) ) ;
#13606 = CARTESIAN_POINT ( 'NONE',  ( 1.430961520682887400, 16.89318350835024063, -220.3256763723340157 ) ) ;
#13607 = CARTESIAN_POINT ( 'NONE',  ( 10.59985392024617745, -10.68425835910226418, -232.2123170752960277 ) ) ;
#13608 = CARTESIAN_POINT ( 'NONE',  ( 14.65870393774896030, -26.09170264574407838, -221.2973805112574723 ) ) ;
#13609 = ORIENTED_EDGE ( 'NONE', *, *, #3964, .F. ) ;
#13610 = CARTESIAN_POINT ( 'NONE',  ( -14.22255565734842619, 21.32307452572284134, -218.8849463683180261 ) ) ;
#13611 = CARTESIAN_POINT ( 'NONE',  ( -15.37153448429513602, 5.014568651886798456, -224.5085656291724945 ) ) ;
#13612 = CARTESIAN_POINT ( 'NONE',  ( 26.92457506054779515, 6.538608665672222209, -219.8654465082432807 ) ) ;
#13613 = ORIENTED_EDGE ( 'NONE', *, *, #65, .F. ) ;
#13614 = CARTESIAN_POINT ( 'NONE',  ( -11.76273268715550913, -21.77324546118368787, -230.3967548854103313 ) ) ;
#13615 = FACE_OUTER_BOUND ( 'NONE', #12832, .T. ) ;
#13616 = ORIENTED_EDGE ( 'NONE', *, *, #17888, .T. ) ;
#13617 = CARTESIAN_POINT ( 'NONE',  ( 11.20580770355584299, 27.81589616365139150, -231.3138133330081132 ) ) ;
#13618 = CARTESIAN_POINT ( 'NONE',  ( 13.95302107590712737, -11.87212821339389812, -220.3052895324516385 ) ) ;
#13619 = CARTESIAN_POINT ( 'NONE',  ( 4.730976410881341465, 17.65764351829336931, -217.6025626048331674 ) ) ;
#13620 = CARTESIAN_POINT ( 'NONE',  ( -21.89482327431018760, 1.733733432562314158, -233.1353281693111796 ) ) ;
#13621 = ADVANCED_FACE ( 'NONE', ( #3304 ), #1944, .T. ) ;
#13622 = TOROIDAL_SURFACE ( 'NONE', #2821, 12.50000000000000355, 5.000000000000000000 ) ;
#13623 = CARTESIAN_POINT ( 'NONE',  ( 23.07558131619435571, 16.33594519118144817, -217.0553921114837124 ) ) ;
#13624 = CARTESIAN_POINT ( 'NONE',  ( -15.46752262371512820, 15.15798787883389487, -233.5981584775992701 ) ) ;
#13625 = CARTESIAN_POINT ( 'NONE',  ( -2.817219543927646175, 14.13981714106644993, -229.6779615865167443 ) ) ;
#13626 = CARTESIAN_POINT ( 'NONE',  ( 16.64225601860865211, 1.926018578292457928, -220.2177910260893725 ) ) ;
#13627 = CARTESIAN_POINT ( 'NONE',  ( 6.131461862964278531, -15.14974102410872625, -231.6805438559109973 ) ) ;
#13628 = CARTESIAN_POINT ( 'NONE',  ( 26.48152825632016061, -2.044474411990439666, -219.3412966555575565 ) ) ;
#13629 = DIRECTION ( 'NONE',  ( 0.000000000000000000, 0.000000000000000000, -1.000000000000000000 ) ) ;
#13630 = PLANE ( 'NONE',  #5115 ) ;
#13631 = CARTESIAN_POINT ( 'NONE',  ( 16.91879448796214191, 0.8271603773820436212, -230.0510230802265710 ) ) ;
#13632 = CARTESIAN_POINT ( 'NONE',  ( -15.89829452305285606, -16.08449805557013335, -231.9408725418336701 ) ) ;
#13633 = CARTESIAN_POINT ( 'NONE',  ( 21.91452165549922881, 0.08546329518220173449, -228.0000000000000853 ) ) ;
#13634 = CARTESIAN_POINT ( 'NONE',  ( 6.679827377097204533, -23.59744646493245668, -231.8618301756397670 ) ) ;
#13635 = CARTESIAN_POINT ( 'NONE',  ( -13.81390866287826746, 1.832988708064121175, -224.4361041349432639 ) ) ;
#13636 = CARTESIAN_POINT ( 'NONE',  ( -0.1881941282075867139, 17.37563936270229092, -230.9177995227891813 ) ) ;
#13637 = CARTESIAN_POINT ( 'NONE',  ( -16.58369694688956741, 24.75758513462668375, -230.3405478298966784 ) ) ;
#13638 = ORIENTED_EDGE ( 'NONE', *, *, #7496, .T. ) ;
#13639 = CARTESIAN_POINT ( 'NONE',  ( -16.74998343472315199, -3.152285961911668988, -228.0274629056708022 ) ) ;
#13640 = ORIENTED_EDGE ( 'NONE', *, *, #14385, .T. ) ;
#13641 = CARTESIAN_POINT ( 'NONE',  ( 10.78187269046063435, 10.73871010366167944, -221.9206544238666368 ) ) ;
#13642 = CARTESIAN_POINT ( 'NONE',  ( -23.30382222616342247, 9.914163031146200566, -218.5285240371296425 ) ) ;
#13643 = CARTESIAN_POINT ( 'NONE',  ( -14.08236938285573636, 6.062428076406559008, -221.7923619418395447 ) ) ;
#13644 = CARTESIAN_POINT ( 'NONE',  ( 0.000000000000000000, 0.000000000000000000, -77.51594804401857175 ) ) ;
#13645 = CARTESIAN_POINT ( 'NONE',  ( 22.73582563804385970, 20.20868311426415431, -227.8513184012435886 ) ) ;
#13646 = CARTESIAN_POINT ( 'NONE',  ( -16.04492519386327487, 1.819644280589142626, -223.4665098021627614 ) ) ;
#13647 = CARTESIAN_POINT ( 'NONE',  ( 2.276720224425493821, 13.44951395023989171, -229.9230017221896105 ) ) ;
#13648 = CARTESIAN_POINT ( 'NONE',  ( 22.42095341476093040, 9.457779162868732215, -232.6339572190428555 ) ) ;
#13649 = EDGE_CURVE ( 'NONE', #3862, #8296, #20257, .T. ) ;
#13650 = CARTESIAN_POINT ( 'NONE',  ( -11.54310632260721903, -10.65784888458977697, -232.4489430773787149 ) ) ;
#13651 = ORIENTED_EDGE ( 'NONE', *, *, #3080, .T. ) ;
#13652 = CARTESIAN_POINT ( 'NONE',  ( -14.26331330459994540, -11.99770975811722451, -232.1846756268951708 ) ) ;
#13653 = CARTESIAN_POINT ( 'NONE',  ( -7.329856113536736828, 10.17606210583481818, -226.3085553030691415 ) ) ;
#13654 = CARTESIAN_POINT ( 'NONE',  ( 5.434900225474387447, -11.93567727083262042, -224.7511004068755369 ) ) ;
#13655 = CARTESIAN_POINT ( 'NONE',  ( 0.6364901924797052857, 13.89978473517355617, -221.8840706290426397 ) ) ;
#13656 = CARTESIAN_POINT ( 'NONE',  ( 11.97659261343968851, -3.740017786417877854, -223.6042415182018033 ) ) ;
#13657 = CARTESIAN_POINT ( 'NONE',  ( -28.55814054826834791, -1.660722980825670048, -228.2640858091212408 ) ) ;
#13658 = CARTESIAN_POINT ( 'NONE',  ( 12.79953165872901266, 10.20044330008568778, -230.3912386799665626 ) ) ;
#13659 = DIRECTION ( 'NONE',  ( 1.224646799147353207E-16, 1.000000000000000000, -0.000000000000000000 ) ) ;
#13660 = CARTESIAN_POINT ( 'NONE',  ( -0.3589900283600636066, 18.35437183075527656, -220.3960288481451357 ) ) ;
#13661 = CARTESIAN_POINT ( 'NONE',  ( 12.63974878616558328, 15.03448928898568759, -231.7036488814491406 ) ) ;
#13662 = CARTESIAN_POINT ( 'NONE',  ( 12.71450444683213021, 7.595266944807587350, -224.4213778964231665 ) ) ;
#13663 = CARTESIAN_POINT ( 'NONE',  ( 26.51393280883522863, 15.12455065102723495, -226.1955201378414415 ) ) ;
#13664 = CARTESIAN_POINT ( 'NONE',  ( 6.679393088666140343, -31.31585170264869689, -224.7195491891107793 ) ) ;
#13665 = CARTESIAN_POINT ( 'NONE',  ( -11.55316006017064012, 19.79513644261079719, -232.3088878043970453 ) ) ;
#13666 = CARTESIAN_POINT ( 'NONE',  ( 24.58316096239279602, 5.861425670879941485, -231.3104446318280623 ) ) ;
#13667 = ADVANCED_BREP_SHAPE_REPRESENTATION ( '', ( #21321, #6677 ), #10599 ) ;
#13668 = CARTESIAN_POINT ( 'NONE',  ( 14.02967383842077709, -23.07461891086659378, -219.7428183145782725 ) ) ;
#13669 = CARTESIAN_POINT ( 'NONE',  ( -11.05032764129755840, 11.65053160594169945, -221.1796278216217218 ) ) ;
#13670 = CARTESIAN_POINT ( 'NONE',  ( 10.31623634631035991, 26.83927646318382898, -220.2315638557092541 ) ) ;
#13671 = CARTESIAN_POINT ( 'NONE',  ( -14.76273180397945772, -6.370707202906876532, -220.0066229284273334 ) ) ;
#13672 = CARTESIAN_POINT ( 'NONE',  ( -16.37512411505367282, 2.406627362596846620, -227.7341547288202719 ) ) ;
#13673 = CARTESIAN_POINT ( 'NONE',  ( 9.851209273476317918, 25.48401176094959553, -233.7173763849377792 ) ) ;
#13674 = ORIENTED_EDGE ( 'NONE', *, *, #8052, .F. ) ;
#13675 = CARTESIAN_POINT ( 'NONE',  ( 10.85888002857596923, 15.81835858589122878, -232.3913150909872627 ) ) ;
#13676 = CARTESIAN_POINT ( 'NONE',  ( 15.93530172229541364, -10.24337635388110890, -230.8272463582829630 ) ) ;
#13677 = CARTESIAN_POINT ( 'NONE',  ( 24.57161139520042781, -7.530326316930160857, -232.9949629211864419 ) ) ;
#13678 = DIRECTION ( 'NONE',  ( -0.000000000000000000, 0.000000000000000000, -1.000000000000000000 ) ) ;
#13679 = CARTESIAN_POINT ( 'NONE',  ( 3.449504654906655254, 27.59247159270940841, -231.3461799890608859 ) ) ;
#13680 = CARTESIAN_POINT ( 'NONE',  ( -30.26911233660276679, -7.575179034252494503, -222.6017624672529109 ) ) ;
#13681 = CARTESIAN_POINT ( 'NONE',  ( -5.519971913460887336, -12.21762732219001713, -227.2962593638428359 ) ) ;
#13682 = CARTESIAN_POINT ( 'NONE',  ( 5.953549895739506326, -12.70069413479034104, -221.3143591192976203 ) ) ;
#13683 = CARTESIAN_POINT ( 'NONE',  ( -21.72273972318264867, 21.08396222359856864, -224.0477214759881690 ) ) ;
#13684 = CARTESIAN_POINT ( 'NONE',  ( 5.066530254613678785, 15.76189963344335254, -222.1234037505291781 ) ) ;
#13685 = CARTESIAN_POINT ( 'NONE',  ( -16.65698539163286540, 11.03290537638306112, -233.6474915129378758 ) ) ;
#13686 = CARTESIAN_POINT ( 'NONE',  ( -27.05172747931452903, 14.36075930490012276, -228.5082213655825853 ) ) ;
#13687 = CARTESIAN_POINT ( 'NONE',  ( -17.67448836398429890, -11.08962652971676199, -218.7915233441472367 ) ) ;
#13688 = ORIENTED_EDGE ( 'NONE', *, *, #20520, .T. ) ;
#13689 = CARTESIAN_POINT ( 'NONE',  ( -4.855966894080006035, 26.75753167227873064, -230.1547293463117114 ) ) ;
#13690 = CARTESIAN_POINT ( 'NONE',  ( 12.23284375931666013, 4.108221165122169616, -224.0993108960438462 ) ) ;
#13691 = CARTESIAN_POINT ( 'NONE',  ( 5.434119414999338815, 11.18343085245738777, -221.0450680983404936 ) ) ;
#13692 = EDGE_CURVE ( 'NONE', #7333, #3760, #13453, .T. ) ;
#13693 = CARTESIAN_POINT ( 'NONE',  ( 24.05238142633148968, -17.07083877791421500, -221.4615098029387070 ) ) ;
#13695 = DIRECTION ( 'NONE',  ( 0.000000000000000000, 0.000000000000000000, -1.000000000000000000 ) ) ;
#13694 = AXIS2_PLACEMENT_3D ( 'NONE', #19841, #19630, #16376 ) ;
#13696 = ORIENTED_EDGE ( 'NONE', *, *, #8783, .F. ) ;
#13697 = CARTESIAN_POINT ( 'NONE',  ( -4.620781219515533778, 16.99182040716223696, -217.1278208835672672 ) ) ;
#13698 = EDGE_CURVE ( 'NONE', #18856, #5014, #6356, .T. ) ;
#13699 = CARTESIAN_POINT ( 'NONE',  ( -17.45568254742804370, -7.678338623619185732, -234.9220303918225738 ) ) ;
#13700 = PLANE ( 'NONE',  #61 ) ;
#13701 = CARTESIAN_POINT ( 'NONE',  ( 15.61962121506769385, 4.525360868525488911, -229.0684696061408090 ) ) ;
#13702 = CARTESIAN_POINT ( 'NONE',  ( -25.29098058636142810, 5.014641116111857144, -217.4658967307323110 ) ) ;
#13703 = CARTESIAN_POINT ( 'NONE',  ( 10.10435529162921853, -13.32996982371095918, -231.5224098423250894 ) ) ;
#13704 = FILL_AREA_STYLE ('',( #6489 ) ) ;
#13705 = CARTESIAN_POINT ( 'NONE',  ( -14.10849459794400751, -0.2436790717799666162, -223.1085195285415921 ) ) ;
#13706 = CARTESIAN_POINT ( 'NONE',  ( -26.58771759052039485, 5.114955214121561511, -218.2823714869195442 ) ) ;
#13707 = CARTESIAN_POINT ( 'NONE',  ( -0.6703493356118243041, -28.01673786290986712, -221.2203946787553548 ) ) ;
#13708 = CARTESIAN_POINT ( 'NONE',  ( 1.526556658859591000E-13, -22.63401512838754570, 77.51594804401857175 ) ) ;
#13709 = DIRECTION ( 'NONE',  ( -1.000000000000000000, 0.000000000000000000, 0.000000000000000000 ) ) ;
#13710 = DIRECTION ( 'NONE',  ( -1.000000000000000000, 0.000000000000000000, 0.000000000000000000 ) ) ;
#13711 = CARTESIAN_POINT ( 'NONE',  ( 18.46162736253148395, -12.23454570505295358, -218.9425382959138062 ) ) ;
#13712 = CARTESIAN_POINT ( 'NONE',  ( 14.66528321205121976, -2.062017816318827190, -227.1804948401301374 ) ) ;
#13713 = CYLINDRICAL_SURFACE ( 'NONE', #5854, 2.000000000000000000 ) ;
#13714 = CARTESIAN_POINT ( 'NONE',  ( 16.48099188159542194, 16.04875567542346815, -230.8408106201084706 ) ) ;
#13715 = CARTESIAN_POINT ( 'NONE',  ( 1.313727069624702981, 17.80710275190598324, -219.4197901500037062 ) ) ;
#13716 = CARTESIAN_POINT ( 'NONE',  ( 20.77649313750695370, -15.65279155457156435, -215.5859610257211898 ) ) ;
#13717 = EDGE_CURVE ( 'NONE', #9167, #3682, #3086, .T. ) ;
#13718 = CARTESIAN_POINT ( 'NONE',  ( 8.649266908999912573, -10.50942778440553482, -226.4415026780416440 ) ) ;
#13719 = VERTEX_POINT ( 'NONE', #21653 ) ;
#13720 = CARTESIAN_POINT ( 'NONE',  ( -8.030397104878142400, 15.90963402996711373, -230.6518438502475590 ) ) ;
#13721 = CARTESIAN_POINT ( 'NONE',  ( -23.99493126334580850, 6.052326449358573335, -219.7958990219547672 ) ) ;
#13722 = CARTESIAN_POINT ( 'NONE',  ( 15.88536911906737181, 12.85343532334862893, -218.9532478288372204 ) ) ;
#13723 = CARTESIAN_POINT ( 'NONE',  ( -9.501265986711061373, -18.16888683615402300, -230.9326763462221948 ) ) ;
#13724 = CARTESIAN_POINT ( 'NONE',  ( -10.76794919243112325, 1.318693451189210089E-15, 92.00000000000000000 ) ) ;
#13725 = ORIENTED_EDGE ( 'NONE', *, *, #5496, .F. ) ;
#13726 = CARTESIAN_POINT ( 'NONE',  ( 22.44730228620155899, 3.608729811217749717, -232.0798239124179645 ) ) ;
#13727 = CARTESIAN_POINT ( 'NONE',  ( 12.24130115618514125, -19.65891960071846967, -230.7381047918825914 ) ) ;
#13728 = CARTESIAN_POINT ( 'NONE',  ( 5.169766346882679997, 29.28517558595074988, -221.5178724947562614 ) ) ;
#13729 = CARTESIAN_POINT ( 'NONE',  ( -15.58461825850822180, 18.91734573546571951, -233.7691177939990723 ) ) ;
#13730 = VECTOR ( 'NONE', #4793, 1000.000000000000000 ) ;
#13731 = CARTESIAN_POINT ( 'NONE',  ( 26.50744623559791435, 1.694095366541529923, -217.6968951254705473 ) ) ;
#13732 = EDGE_CURVE ( 'NONE', #6741, #237, #19548, .T. ) ;
#13733 = CIRCLE ( 'NONE', #16597, 21.80000000000000071 ) ;
#13734 = CARTESIAN_POINT ( 'NONE',  ( -6.571166997218196748, 12.74865329367398736, -229.9840124400968762 ) ) ;
#13735 = CARTESIAN_POINT ( 'NONE',  ( -3.400000000000003908, 0.000000000000000000, -224.9999999999999716 ) ) ;
#13736 = CARTESIAN_POINT ( 'NONE',  ( -3.734153817218577309, -19.72686645808614614, -233.9207428641194610 ) ) ;
#13737 = DIRECTION ( 'NONE',  ( -0.000000000000000000, -0.000000000000000000, 1.000000000000000000 ) ) ;
#13738 = FACE_OUTER_BOUND ( 'NONE', #20511, .T. ) ;
#13739 = PRODUCT_DEFINITION_SHAPE ( 'NONE', 'NONE',  #22269 ) ;
#13740 = CARTESIAN_POINT ( 'NONE',  ( -23.84209965496292227, -7.976777114481962805, -232.1458837748831456 ) ) ;
#13742 = CARTESIAN_POINT ( 'NONE',  ( -13.09048442463468120, -0.002406630494250819839, -229.7150300986316438 ) ) ;
#13741 = B_SPLINE_CURVE_WITH_KNOTS ( 'NONE', 3,
 ( #8758, #20883, #18982, #15953, #10439, #13937, #5469, #17532, #7068, #12469 ),
 .UNSPECIFIED., .F., .F.,
 ( 4, 2, 2, 2, 4 ),
 ( 0.4925451859516016828, 0.4926212833915588618, 0.4960388740592901469, 0.4979917830122794764, 0.4999446919652688059 ),
 .UNSPECIFIED. ) ;
#13743 = CARTESIAN_POINT ( 'NONE',  ( -15.00281653375496127, -15.21317112889928858, -231.9690514080965613 ) ) ;
#13744 = AXIS2_PLACEMENT_3D ( 'NONE', #20820, #2037, #3385 ) ;
#13745 = SURFACE_SIDE_STYLE ('',( #20359 ) ) ;
#13746 = CARTESIAN_POINT ( 'NONE',  ( 13.60960062514055657, -26.18013421850907108, -225.9721930653775246 ) ) ;
#13747 = CARTESIAN_POINT ( 'NONE',  ( 22.16968511661519869, 1.542591969257184337, -234.6098499860488573 ) ) ;
#13748 = CARTESIAN_POINT ( 'NONE',  ( -1.772400894765090662, 19.49811434610897010, -217.8797837662441168 ) ) ;
#13749 = CARTESIAN_POINT ( 'NONE',  ( -9.439286754415764591, 28.32957437491962338, -228.7842975624562598 ) ) ;
#13750 = CARTESIAN_POINT ( 'NONE',  ( 22.56961104628404868, -1.854966590244772950, -214.8717168148014025 ) ) ;
#13751 = CARTESIAN_POINT ( 'NONE',  ( 15.91295838535984331, 21.88410254487826379, -230.9583961155862823 ) ) ;
#13752 = CARTESIAN_POINT ( 'NONE',  ( -16.88427011841620029, 9.219900108593305887, -231.9155403335099948 ) ) ;
#13753 = CARTESIAN_POINT ( 'NONE',  ( -19.84402263676350131, 8.565754689849573111, -217.6561116767911983 ) ) ;
#13754 = CARTESIAN_POINT ( 'NONE',  ( -15.95714424191699266, -19.90201571590360885, -231.7641511196865451 ) ) ;
#13755 = AXIS2_PLACEMENT_3D ( 'NONE', #15857, #12253, #19219 ) ;
#13756 = CARTESIAN_POINT ( 'NONE',  ( 0.000000000000000000, -17.50000000000000711, -60.00000000000000000 ) ) ;
#13757 = CARTESIAN_POINT ( 'NONE',  ( 30.52813181070726856, 5.438803974502569361, -223.5441926215666513 ) ) ;
#13758 = CARTESIAN_POINT ( 'NONE',  ( -16.54465188417290022, 6.134005835925411709, -228.8256222654843270 ) ) ;
#13759 = CARTESIAN_POINT ( 'NONE',  ( 13.79814099039094089, 16.09927043668092850, -214.6489469124405502 ) ) ;
#13760 = CARTESIAN_POINT ( 'NONE',  ( 13.06625079052675531, 10.14096931681969238, -232.1435240729728093 ) ) ;
#13761 = CARTESIAN_POINT ( 'NONE',  ( -5.974374721719333259, -11.49502099717533454, -225.7652523315031488 ) ) ;
#13762 = CIRCLE ( 'NONE', #1173, 3.000000000000002665 ) ;
#13763 = ORIENTED_EDGE ( 'NONE', *, *, #20966, .F. ) ;
#13764 = CARTESIAN_POINT ( 'NONE',  ( -4.994543945659216000, -15.01629888130124435, -221.3392717856295633 ) ) ;
#13765 = CARTESIAN_POINT ( 'NONE',  ( -6.079211283031130897, 16.94466709905296753, -232.9163774423793711 ) ) ;
#13766 = CARTESIAN_POINT ( 'NONE',  ( 6.741123954526870854, -14.00899218320067341, -219.0418835583997179 ) ) ;
#13767 = CARTESIAN_POINT ( 'NONE',  ( -11.42613629117093765, 28.09170287990588832, -228.7150250545069241 ) ) ;
#13768 = CARTESIAN_POINT ( 'NONE',  ( 23.46500920064399409, -11.67104692860896620, -233.8722294412333724 ) ) ;
#13769 = CARTESIAN_POINT ( 'NONE',  ( -17.58118739749173898, -8.238107657346720458, -217.5252134542318458 ) ) ;
#13770 = CARTESIAN_POINT ( 'NONE',  ( -24.15814485343234352, 4.373587128574028426, -232.6698675874553430 ) ) ;
#13771 = DIRECTION ( 'NONE',  ( -0.000000000000000000, -0.000000000000000000, -1.000000000000000000 ) ) ;
#13772 = CARTESIAN_POINT ( 'NONE',  ( -5.560972518124746244, 14.60655266358653215, -227.5460946431043681 ) ) ;
#13773 = CARTESIAN_POINT ( 'NONE',  ( 21.17011458613547248, 1.652544727609948527, -234.6098499860487152 ) ) ;
#13774 = CARTESIAN_POINT ( 'NONE',  ( 17.99029889091409018, 9.613712288440757092, -232.0298403238024036 ) ) ;
#13775 = CARTESIAN_POINT ( 'NONE',  ( 29.01678366425524658, 8.126504218505314014, -229.6975090854573125 ) ) ;
#13776 = CARTESIAN_POINT ( 'NONE',  ( -0.07228948136920625156, -12.49432715273631445, -224.3346527204968766 ) ) ;
#13777 = CARTESIAN_POINT ( 'NONE',  ( 5.964915545484365644, 11.50358694729900577, -229.9646467236423462 ) ) ;
#13778 = AXIS2_PLACEMENT_3D ( 'NONE', #13644, #4851, #5071 ) ;
#13779 =( BOUNDED_SURFACE ( )  B_SPLINE_SURFACE ( 3, 3, ( 
 ( #20100, #4689, #11563, #16972, #18438, #3336, #10218, #9884, #12018, #16748, #8539, #8427, #13601, #15403, #17087, #15070, #21908, #7406, #17300, #1770, #15505, #19316, #419, #6956, #7293, #12238, #21108, #2099, #7183, #12573, #14276, #19417, #14165, #4001, #312, #20773, #7069, #8979, #8871, #17420, #21000, #10440, #5693, #5355, #13938, #2205, #1989, #13828, #14048, #85, #9085, #5590, #20664, #5246, #12128, #17193, #15735, #18983, #12470, #3895, #8644, #3562, #1875, #17638, #20884, #5470, #15954, #12354, #19204, #528, #8759, #15619, #200, #19089, #10772, #3665, #10551, #3785, #10667, #17533, #15843, #852, #6247, #1073, #13121, #7840, #19967, #16276, #12681, #4224, #16066, #9412, #2753, #19639, #14706, #7947, #2647, #9528, #11209, #7729, #14600, #21541, #637, #14380, #21435, #14811, #7513, #5916, #10995, #19851, #19746, #10876, #18075, #966, #6131, #11103, #17754, #2535, #13005, #16171, #2317, #6025, #11321, #21320, #19530, #21214, #9203, #17971, #12899, #17865, #4326, #4438, #16387, #16496, #18190, #9634, #5800, #21654, #4116, #2427, #9310, #741, #7617, #14485, #12793, #4662, #15265, #9970, #1298, #17058, #18408, #9742, #11535, #3305, #18738, #9856, #8512, #1185, #20294, #18299, #10078, #22222, #20179, #21990, #10188, #8279, #15375, #2858, #1635, #2970, #22115, #16829, #8172, #6813, #16721, #16604, #15038, #13679, #4554, #21879, #11430, #8064, #4889, #14929, #16943, #21768, #4773, #6468, #13337, #11769, #18521, #11650, #1519, #20075, #6357, #3087, #1407, #11874, #15148, #13229, #6583, #13454, #18633, #8397, #3195, #6702, #13573, #20409, #4998, #10302, #17503, #15814, #7377, #10744, #5105, #20970, #5327, #12209, #12436, #10518, #8840, #19287, #17610, #20634, #11986, #18847, #391, #3751, #17165, #10636, #15589, #2176, #5438, #17386, #15923, #9057, #501, #2070, #20515, #3637, #51, #13911, #3422, #19062, #3864, #7039, #8950, #1743, #12320, #19174, #20854, #1962, #15706, #7262, #8617, #15477, #283, #6924, #13793, #170, #5219, #14132, #7152, #12100, #5558, #18955, #3531, #20746, #10411, #14018, #17272, #1846, #8724, #17941, #14677, #2397, #16036, #19390, #1045, #7586, #2505, #21184, #5884, #11179, #9383, #19822, #21511, #14455, #14245, #21288, #6102, #9280, #19610, #4195, #16356, #12543, #18160, #7483, #16245, #7812, #5770, #4407, #18046, #16140, #11289, #21078, #17833, #19716, #712, #12760, #11073, #9173, #7699, #12974, #820, #14568, #608, #21405, #5995, #2725, #9496, #2615, #12868, #16468, #19497, #14352, #4085, #9606, #5665, #3973, #4297, #10847, #17721, #934, #12651, #2287 ),
 ( #10962, #3277, #20379, #10162, #4862, #17031, #13307, #9714, #1268, #13090, #6438, #22082, #16688, #11739, #4973, #21960, #6553, #8254, #20149, #4742, #18607, #19936, #11402, #18493, #11848, #4524, #2940, #8032, #16915, #16803, #7918, #15121, #20266, #3169, #8144, #14781, #21849, #10052, #13202, #21623, #11621, #8367, #18376, #16575, #18271, #6215, #15009, #3053, #14898, #9943, #1489, #1378, #13544, #15237, #13425, #2832, #6672, #18713, #1156, #21737, #6329, #20047, #4634, #11508, #9827, #12290, #7007, #20604, #14103, #15453, #6784, #1717, #367, #15788, #19142, #10718, #20940, #8484, #2044, #8693, #15559, #7234, #13879, #12180, #5527, #12406, #8592, #15348, #22196, #3722, #7123, #13653, #13990, #18929, #19257, #8812, #20717, #3837, #1606, #20488, #20826, #5079, #5298, #3393, #17244, #11960, #139, #18821, #10383, #5407, #10275, #15675, #255, #1932, #19034, #3611, #10604, #17141, #25, #10489, #6895, #13765, #3504, #5190, #17473, #17355, #12072, #8922, #1815, #12848, #4059, #17584, #9255, #5971, #581, #19797, #21263, #18022, #5744, #19365, #474, #4381, #10934, #5856, #2261, #16114, #14545, #12737, #908, #2589, #17807, #2150, #2372, #9472, #19582, #16332, #4171, #21487, #15894, #7788, #17692, #19690, #687, #14324, #14654, #9144, #7348, #16005, #6078, #12953, #7456, #9030, #14214, #11049, #21049, #795, #5639, #7562, #21156, #12624, #2479, #14430, #17915, #7675, #10822, #12515, #19470, #9361, #3946, #16220, #21381, #4276, #11156, #18881, #15407, #14757, #16447, #21597, #20668, #3228, #1020, #8544, #2701, #4500, #6737, #10223, #10335, #15509, #7897, #2810, #21713, #18352, #6960, #90, #3456, #6188, #13180, #3340, #1128, #11266, #14872, #10111, #17091, #8004, #1669, #18248, #18135, #1774, #18772, #13832, #11485, #6305, #17198, #9584, #8648, #20023, #13067, #11907, #1556, #19911, #11379, #9689, #16550, #4610, #16976, #8431, #15298, #22148, #13605, #22253, #20442, #5031, #6846, #13714, #20552, #5140, #12022, #15623, #14052, #17643, #12132, #14384, #19319, #640, #15739, #10672, #17537, #7408, #3567, #9207, #20777, #423, #21112, #19093, #17758, #2209, #7186, #10882, #5252, #8875, #10775, #317, #20888, #5475, #204, #21003, #19420, #2103, #12358, #7074, #8984, #19208, #16070, #531, #9091, #15847, #7516, #10554, #5359, #17424, #2322, #18987, #4006, #3899, #10444, #17304, #3789, #12243, #12474, #7298, #14168, #1880, #5697, #5593, #8763, #15958, #3670, #1993, #14278, #13943, #12577, #14710, #2651, #9638, #4228, #21218, #16609, #21545, #4558, #19857, #1191, #19643, #19971, #9417, #11434, #5920 ),
 ( #9314, #7734, #11325, #5805, #8068, #13010, #12686, #16282, #4330, #11214, #1077, #19533, #2862, #14491, #16392, #14816, #12797, #18303, #18194, #856, #9746, #4120, #2539, #4442, #14604, #21439, #6029, #16175, #6136, #13125, #18081, #12903, #745, #9532, #19750, #11001, #16500, #2757, #970, #17869, #11107, #21326, #17975, #2431, #7622, #7844, #7951, #21661, #6251, #13458, #8176, #22119, #6589, #3199, #3426, #15379, #9974, #20079, #20413, #13341, #15042, #4779, #17169, #21883, #8402, #18637, #3309, #20183, #14933, #10306, #15269, #20519, #13577, #6361, #6472, #10082, #5002, #13683, #18851, #4666, #11654, #3091, #21994, #1747, #21772, #22226, #11539, #16834, #6706, #18525, #13233, #1411, #20298, #11878, #8283, #18742, #15152, #18413, #5109, #10194, #2976, #4893, #11773, #11991, #9860, #16725, #16947, #6817, #17062, #1523, #1302, #1639, #8516, #3977, #19066, #14022, #20858, #10748, #6928, #12547, #1850, #3755, #2180, #174, #21082, #5563, #10522, #14249, #17725, #12213, #14136, #3641, #17392, #1966, #3535, #2074, #505, #5442, #8844, #10415, #12324, #15710, #19394, #3868, #12441, #19179, #10851, #13915, #8728, #20750, #5669, #8621, #7381, #395, #15482, #13799, #7156, #15595, #15818, #287, #10640, #55, #9061, #17507, #20638, #20975, #7043, #5331, #8954, #5223, #7266, #19291, #17614, #15927, #12104, #18959, #17276, #18050, #7922, #938, #16040, #17837, #19721, #7816, #1049, #6219, #14356, #16144, #12766, #9387, #19942, #13094, #9610, #7487, #4199, #16362, #14459, #11406, #5888, #16249, #14681, #21292, #21515, #9284, #2292, #14786, #9500, #4529, #2509, #19614, #21627, #9177, #612, #11078, #16472, #2619, #14573, #21189, #5774, #12655, #716, #19501, #17945, #4090, #7590, #10967, #824, #6107, #5999, #2402, #7703, #21409, #12872, #4301, #11183, #12978, #19826, #4411, #11294, #18166, #2729, #20385, #16579, #22201, #11512, #13429, #11853, #9831, #8490, #15242, #20153, #1611, #5084, #21853, #1494, #13311, #4746, #11625, #13206, #11744, #10167, #1383, #18497, #20051, #15125, #3059, #6790, #13549, #22087, #8258, #20494, #1274, #18381, #8148, #15354, #13658, #17036, #10057, #18275, #1160, #16807, #2944, #3173, #9947, #6557, #2836, #18718, #21964, #8036, #8372, #16692, #15013, #6442, #9718, #20270, #18611, #4867, #6678, #16920, #14902, #21743, #4978, #6333, #3282, #4638, #5195, #7128, #10609, #10723, #15899, #1723, #3509, #144, #19040, #7353, #479, #19263, #17146, #13886, #3727, #1821, #21056, #15564, #3616, #17480, #8698, #2049, #18934, #11965, #2155, #19149, #14220, #12185, #7012, #17589, #18826 ),
 ( #3843, #5303, #3398, #10495, #9035, #13995, #10281, #15682, #8597, #15459, #31, #12078, #372, #17360, #20722, #6900, #10389, #13770, #17249, #20609, #1937, #8817, #8927, #260, #20831, #5413, #12295, #15793, #7239, #14108, #20945, #5533, #12411, #19695, #4282, #5977, #4177, #17921, #9477, #10826, #9149, #16225, #9590, #2265, #692, #5749, #14659, #14550, #1025, #12853, #18027, #913, #14435, #5644, #19587, #16337, #10939, #7902, #9366, #6083, #16119, #7461, #17697, #14762, #21269, #801, #12629, #11054, #2595, #7680, #11271, #12959, #5861, #12521, #12742, #19802, #21386, #4387, #11161, #16452, #3951, #18140, #19475, #7794, #2485, #2377, #2706, #4064, #16010, #17812, #19370, #587, #9261, #14329, #21162, #21492, #7568, #1360, #15216, #9806, #20028, #13185, #3035, #8124, #16670, #8233, #1134, #1468, #4615, #11490, #18586, #1250, #11384, #6419, #19916, #3148, #15103, #18253, #4504, #2815, #6649, #14989, #9694, #21939, #6531, #21603, #8345, #6195, #10032, #21830, #13289, #16894, #20130, #11600, #22060, #13073, #2920, #8012, #14877, #16555, #21718, #18357, #6310, #4719, #18472, #9921, #16785, #13401, #20245, #4839, #11716, #5206, #6691, #10179, #13444, #18511, #3294, #18945, #11640, #10069, #15138, #1734, #1624, #10400, #22212, #5096, #10293, #1508, #15029, #13564, #3412, #20284, #17260, #18729, #15469, #3185, #16820, #20169, #1833, #8388, #17048, #21979, #20399, #11977, #8502, #20623, #42, #15256, #21869, #22103, #6913, #15366, #13784, #6803, #3520, #13327, #12090, #6573, #17158, #4989, #11759, #6458, #4880, #4763, #18624, #3075, #9961, #16933, #1398, #8271, #13670, #11864, #20505, #18838, #8608, #12307, #20842, #15913, #382, #8937, #14234, #1948, #5760, #19163, #5425, #16023, #15804, #5314, #5546, #13898, #599, #12533, #12196, #20734, #19052, #17825, #7250, #3627, #5656, #3962, #8710, #21173, #15577, #9161, #14121, #20957, #7471, #12424, #19276, #14340, #12640, #8827, #156, #7025, #10837, #21068, #10507, #19381, #3738, #19489, #492, #3854, #4077, #10952, #17373, #17711, #15693, #10734, #270, #2059, #7140, #17599, #14006, #17492, #2278, #10622, #7365, #2166, #9046, #11283, #20040, #9601, #14775, #19929, #11171, #2387, #16351, #13084, #7693, #4627, #6094, #2827, #12863, #4188, #7579, #11501, #18039, #12969, #9376, #926, #21615, #19814, #8024, #9707, #2608, #9272, #9489, #16567, #4399, #1147, #18153, #6321, #703, #14890, #2496, #4515, #7805, #21397, #21730, #16236, #14445, #813, #13195, #16130, #14562, #21280, #5874, #2718, #12753, #7912, #19601, #14670, #5989, #19707, #16463, #21504 ),
 ( #11064, #1038, #6207, #17934, #11395, #18263, #4292, #13646, #15341, #1483, #20596, #1371, #18485, #8247, #15448, #1710, #10269, #10155, #5183, #1261, #16907, #11612, #3270, #10046, #6665, #6888, #18815, #13417, #8136, #1600, #16796, #3047, #15115, #18370, #9934, #11842, #22076, #6777, #21953, #2931, #13758, #18707, #8585, #17024, #9819, #6545, #13536, #8478, #17135, #18, #15002, #16682, #20373, #22189, #21840, #6432, #3387, #13301, #20258, #20482, #20142, #4735, #4854, #11731, #4965, #5073, #18599, #3162, #8360, #15230, #11951, #3831, #1926, #21151, #15669, #19135, #10713, #8806, #17578, #19028, #12066, #2255, #19252, #7450, #12284, #7117, #17686, #575, #9137, #248, #19360, #12400, #2039, #17238, #15999, #14318, #10482, #10817, #13983, #18923, #3605, #3498, #10598, #2145, #15783, #10375, #1809, #8686, #15552, #132, #14096, #7001, #20821, #9025, #13873, #20712, #15888, #5293, #5399, #17468, #8916, #14210, #12173, #17347, #3716, #7229, #5635, #361, #20934, #466, #5522, #7343, #21045, #12511, #3941, #789, #7668, #14538, #682, #21480, #19904, #11150, #21374, #7556, #2583, #5966, #9683, #1013, #2695, #18016, #7998, #11043, #5849, #17909, #2803, #11373, #4493, #19791, #14863, #10928, #4271, #21258, #12946, #19685, #16325, #16543, #6182, #12842, #17800, #11258, #4164, #12731, #2474, #5739, #19576, #6073, #9465, #16440, #9355, #12618, #1121, #4374, #18241, #18127, #19463, #16215, #902, #9577, #7889, #4052, #2367, #9249, #16109, #7782, #14750, #14425, #14648, #13059, #21591, #1349, #13507, #11587, #8560, #3022, #6519, #20345, #18459, #4941, #6408, #21705, #11924, #6637, #17107, #21929, #16771, #5048, #10241, #18792, #9909, #6753, #22047, #11703, #4603, #3359, #1687, #20120, #20459, #8221, #6297, #13278, #13171, #20232, #11817, #3137, #20016, #11478, #18345, #2907, #9792, #1457, #16656, #15092, #18683, #1238, #8112, #3245, #14978, #13388, #4826, #18575, #1576, #21818, #4708, #10019, #16882, #15318, #8331, #15202, #10129, #16996, #8448, #22165, #13623, #20908, #10460, #17322, #1900, #10352, #8893, #7316, #20797, #8782, #17215, #12259, #15643, #19337, #10690, #12376, #5376, #17660, #20688, #15526, #5268, #12490, #21022, #14185, #7204, #2229, #20571, #13959, #8664, #337, #7093, #3689, #3917, #15863, #224, #5158, #5495, #13849, #109, #12148, #15425, #6978, #15758, #19111, #3807, #19006, #8882, #10794, #14071, #5611, #19227, #6863, #3583, #10573, #17442, #13731, #17554, #2122, #2012, #12039, #9000, #441, #18899, #3473, #1788, #988, #877, #11344, #14296, #7640, #2340, #16301, #764, #19660 ),
 ( #21565, #18215, #6046, #4464, #14513, #10901, #2449, #21129, #21345, #7863, #17886, #12921, #6154, #7753, #14624, #9439, #13030, #5938, #4245, #7534, #12594, #11125, #19878, #5716, #4140, #9226, #18102, #17993, #9111, #21457, #19767, #4347, #9332, #15975, #12817, #11231, #14403, #549, #2556, #9552, #19551, #17776, #19439, #7428, #16192, #2669, #16087, #16414, #14728, #4025, #657, #21234, #5826, #12705, #11019, #17264, #20204, #1836, #6491, #7028, #1095, #8714, #2882, #13479, #8195, #21793, #15581, #16628, #7968, #9763, #159, #13902, #8087, #20737, #21679, #18547, #16517, #8305, #5318, #18431, #6379, #14954, #9994, #16744, #2996, #15172, #18321, #12199, #13251, #20096, #10403, #9880, #6270, #21903, #14835, #2775, #6610, #13145, #19990, #9657, #1324, #4577, #15063, #11453, #4800, #1212, #13360, #4684, #11558, #11676, #3114, #20318, #16856, #1432, #22015, #4916, #11792, #18659, #3219, #10954, #2062, #706, #15696, #12536, #10511, #2280, #14448, #12426, #384, #8942, #3965, #10737, #19279, #9163, #12312, #16133, #7252, #15807, #4079, #3856, #274, #15916, #1952, #17827, #601, #7144, #8830, #14009, #5877, #17602, #20846, #16026, #14344, #19055, #9274, #3631, #19492, #2169, #9048, #2390, #494, #7368, #7581, #21283, #19166, #17376, #5428, #21177, #7473, #3741, #5763, #14124, #10626, #10840, #14236, #17495, #20960, #5548, #12644, #21070, #5659, #19383, #17714, #17937, #11285, #4629, #21507, #9709, #9823, #4517, #11397, #13086, #2934, #4403, #7914, #11173, #16238, #1040, #16684, #9379, #7807, #12865, #21732, #21618, #8139, #19931, #2829, #8027, #6097, #12755, #18155, #1151, #18042, #15004, #16465, #13197, #816, #6323, #7695, #20042, #18265, #2720, #2498, #1263, #21842, #2611, #6210, #19603, #16569, #14892, #11504, #12971, #4190, #9603, #18372, #9491, #11067, #14778, #14564, #21399, #5991, #19711, #4294, #19817, #16353, #928, #14672, #3389, #1602, #12068, #13760, #22078, #15554, #6667, #20599, #8480, #5186, #10157, #10377, #4737, #18925, #6547, #17137, #11844, #3164, #3500, #20260, #11615, #13420, #17240, #1811, #11733, #8688, #3049, #22192, #20144, #11953, #6434, #13539, #10048, #18601, #13648, #20375, #4967, #18817, #21955, #13303, #16909, #1485, #18488, #18709, #9936, #3272, #16798, #1373, #10271, #8249, #15117, #4857, #8362, #17027, #15233, #1712, #8588, #15343, #6779, #20484, #6890, #5075, #15450, #20, #12402, #10715, #14320, #12620, #251, #7003, #20714, #2257, #5637, #12176, #12513, #17470, #4054, #7345, #19254, #17802, #19465, #2369, #19362, #9251, #5524, #1928, #15785, #5295, #20936 ),
 ( #468, #135, #10930, #7452, #19030, #2041, #14212, #12286, #13876, #3607, #577, #8919, #10484, #3943, #20823, #7119, #19137, #17349, #13985, #15890, #3833, #10819, #5401, #8808, #15671, #21047, #5741, #17688, #3718, #10601, #17581, #9139, #21153, #363, #7231, #14098, #2147, #16002, #9027, #4605, #1123, #21260, #18018, #7891, #5968, #2909, #19687, #904, #14752, #12844, #21593, #791, #16111, #6300, #1015, #11480, #16327, #11152, #2697, #4166, #2805, #11045, #8000, #16442, #6075, #5851, #20018, #18347, #14540, #14865, #4273, #21707, #7670, #7558, #14650, #6184, #19793, #684, #14427, #12733, #13173, #19578, #18129, #17911, #2585, #13061, #2476, #9357, #19907, #16217, #9467, #21482, #12949, #18243, #21377, #7784, #4376, #11260, #9685, #9579, #4496, #11375, #16545, #15426, #18900, #13391, #15321, #4829, #11706, #18577, #4710, #3247, #1689, #15205, #3139, #11589, #6639, #10022, #13734, #5051, #6755, #22050, #12041, #15094, #9912, #21931, #6864, #6700, #8562, #1578, #9794, #14980, #8334, #3024, #16999, #1459, #20348, #20572, #20234, #6521, #17111, #16884, #6410, #13510, #21820, #5159, #13625, #13280, #20122, #18461, #16658, #4943, #16775, #20461, #11927, #1240, #8115, #1351, #10243, #11819, #18685, #8223, #10132, #8451, #22167, #18794, #3362, #10353, #1789, #5613, #9001, #15528, #15865, #20799, #7429, #10691, #15759, #21130, #15976, #5717, #443, #12596, #8894, #5269, #19113, #8665, #2014, #17661, #12260, #7317, #551, #17555, #2123, #3808, #14297, #17444, #20910, #1901, #6979, #14072, #3475, #111, #5377, #3584, #12491, #12377, #17216, #14187, #21023, #19338, #3690, #13850, #338, #3919, #8784, #20691, #7206, #10795, #12150, #19228, #5497, #2232, #10574, #9112, #10461, #19007, #17324, #15644, #226, #7095, #13960, #6274, #12819, #11349, #14627, #18219, #879, #1099, #17778, #2778, #19554, #7867, #2558, #16194, #9662, #11021, #2342, #4142, #16521, #7974, #2451, #14840, #16089, #12925, #10904, #2673, #21683, #19662, #766, #9334, #4350, #11127, #4248, #9555, #12707, #659, #9229, #7536, #19441, #17995, #14405, #16417, #14731, #4028, #21237, #5829, #19881, #9443, #16304, #17889, #7755, #21459, #7644, #14515, #21347, #5941, #6050, #21570, #993, #19771, #6157, #11235, #18105, #13035, #4468, #8538, #3335, #15402, #10107, #22248, #18551, #14957, #6495, #18325, #11680, #5026, #21907, #16971, #10217, #4920, #11796, #13483, #17086, #4804, #8309, #11562, #16634, #1437, #1663, #9768, #8199, #13255, #22141, #22023, #13148, #20322, #3223, #8426, #13366, #19994, #3118, #1550, #18437, #4580, #16860, #13600 ) ),
 .UNSPECIFIED., .T., .F., .F. ) 
 B_SPLINE_SURFACE_WITH_KNOTS ( ( 4, 3, 4 ),
 ( 4, 2, 2, 2, 2, 2, 2, 2, 2, 2, 2, 2, 2, 2, 2, 2, 2, 2, 2, 2, 2, 2, 2, 2, 2, 2, 2, 2, 2, 2, 2, 2, 2, 2, 2, 2, 2, 2, 2, 2, 2, 2, 2, 2, 2, 2, 2, 2, 2, 2, 2, 2, 2, 2, 2, 2, 2, 2, 2, 2, 2, 2, 2, 2, 2, 2, 2, 2, 2, 2, 2, 2, 2, 2, 2, 2, 2, 2, 2, 2, 2, 2, 2, 2, 2, 2, 2, 2, 2, 2, 2, 2, 2, 2, 2, 2, 2, 2, 2, 2, 2, 2, 2, 2, 2, 2, 2, 2, 2, 2, 2, 2, 2, 2, 2, 2, 2, 2, 2, 2, 2, 2, 2, 2, 2, 2, 2, 2, 2, 2, 2, 2, 2, 2, 2, 2, 2, 2, 2, 2, 2, 2, 2, 2, 2, 2, 2, 2, 2, 2, 2, 2, 2, 2, 2, 2, 2, 2, 2, 2, 2, 2, 2, 2, 2, 2, 2, 4 ),
 ( 0.000000000000000000, 0.5000000000000000000, 1.000000000000000000 ),
 ( 0.000000000000000000, 0.001952908952989333875, 0.003905817905978667751, 0.007323408573709997045, 0.01074099924144132634, 0.01415858990917265650, 0.01586738524303832332, 0.01757618057690398666, 0.02099377124463531682, 0.02441136191236664699, 0.02782895258009797368, 0.03124654324782930384, 0.03466413391556063400, 0.03808172458329196070, 0.04149931525102329433, 0.04491690591875462102, 0.04662570125262028436, 0.04833449658648594771, 0.05175208725421727440, 0.05346088258808293775, 0.05516967792194860110, 0.05858726858967993473, 0.06200485925741126836, 0.06542244992514259505, 0.06884004059287393562, 0.07225763126060526231, 0.07567522192833658901, 0.07909281259606792958, 0.08251040326379925627, 0.08421919859766491268, 0.08592799393153058296, 0.08934558459926195129, 0.09276317526699331961, 0.09447197060085900377, 0.09618076593472468794, 0.09959835660245604239, 0.1030159472701873968, 0.1064335379379187652, 0.1098511286056501335, 0.1132687192733815018, 0.1166863099411127869, 0.1201039006088440858, 0.1235214912765753847, 0.1252302866104410273, 0.1269390819443066698, 0.1303566726120379826, 0.1320654679459036251, 0.1337742632797692677, 0.1371918539475005527, 0.1406094446152318378, 0.1440270352829631784, 0.1474446259506944912, 0.1508622166184258040, 0.1542798072861571446, 0.1576973979538884851, 0.1611149886216198257, 0.1645325792893511663, 0.1679501699570824791, 0.1713677606248137919, 0.1747853512925451325, 0.1764941466264108028, 0.1782029419602764730, 0.1816205326280078136, 0.1850381232957391542, 0.1884557139634704670, 0.1918733046312017798, 0.1952908952989331204, 0.1987084859666644610, 0.2021260766343957738, 0.2055436673021270866, 0.2072524626359927569, 0.2089612579698584272, 0.2123788486375897677, 0.2140876439714554380, 0.2157964393053211083, 0.2192140299730524489, 0.2226316206407837617, 0.2260492113085151300, 0.2294668019762464706, 0.2328843926439778111, 0.2363019833117091517, 0.2397195739794404923, 0.2431371646471718329, 0.2465547553149031734, 0.2499723459826345140, 0.2533899366503657991, 0.2568075273180971396, 0.2602251179858284802, 0.2636427086535597653, 0.2670602993212910503, 0.2704778899890223909, 0.2738954806567537315, 0.2773130713244850165, 0.2807306619922163571, 0.2841482526599476977, 0.2858570479938133957, 0.2875658433276790382, 0.2909834339954103788, 0.2926922293292760768, 0.2944010246631417194, 0.2978186153308730599, 0.3012362059986043450, 0.3046537966663356856, 0.3080713873340670261, 0.3114889780017983112, 0.3149065686695296518, 0.3183241593372609923, 0.3217417500049923329, 0.3234505453388579754, 0.3251593406727236735, 0.3285769313404549585, 0.3319945220081862991, 0.3354121126759176397, 0.3388297033436489247, 0.3422472940113802653, 0.3456648846791116059, 0.3490824753468429464, 0.3525000660145742870, 0.3559176566823056276, 0.3593352473500369682, 0.3627528380177683087, 0.3661704286854996493, 0.3695880193532309343, 0.3730056100209622749, 0.3747144053548279174, 0.3764232006886936155, 0.3798407913564249005, 0.3832583820241562411, 0.3866759726918875817, 0.3900935633596189223, 0.3935111540273502628, 0.3969287446950816034, 0.4003463353628129440, 0.4037639260305442845, 0.4054727213644099271, 0.4071815166982756251, 0.4105991073660069102, 0.4140166980337382507, 0.4157254933676038933, 0.4174342887014695913, 0.4208518793692008764, 0.4242694700369322169, 0.4276870607046635575, 0.4311046513723948981, 0.4345222420401262386, 0.4379398327078575237, 0.4413574233755888643, 0.4447750140433202048, 0.4464838093771859029, 0.4481926047110515454, 0.4516101953787828860, 0.4533189907126485840, 0.4550277860465142266, 0.4584453767142455671, 0.4618629673819769077, 0.4652805580497082483, 0.4686981487174395888, 0.4721157393851709294, 0.4755333300529022145, 0.4789509207206335550, 0.4823685113883648956, 0.4840773067222305381, 0.4857861020560961807, 0.4892036927238275212, 0.4926212833915588618, 0.4960388740592901469, 0.4979917830122794764, 0.4999446919652688059 ),
 .UNSPECIFIED. ) 
 GEOMETRIC_REPRESENTATION_ITEM ( )  RATIONAL_B_SPLINE_SURFACE ( (
 ( 1.000000000000000000, 1.000000000000000000, 1.000000000000000000, 1.000000000000000000, 1.000000000000000000, 1.000000000000000000, 1.000000000000000000, 1.000000000000000000, 1.000000000000000000, 1.000000000000000000, 1.000000000000000000, 1.000000000000000000, 1.000000000000000000, 1.000000000000000000, 1.000000000000000000, 1.000000000000000000, 1.000000000000000000, 1.000000000000000000, 1.000000000000000000, 1.000000000000000000, 1.000000000000000000, 1.000000000000000000, 1.000000000000000000, 1.000000000000000000, 1.000000000000000000, 1.000000000000000000, 1.000000000000000000, 1.000000000000000000, 1.000000000000000000, 1.000000000000000000, 1.000000000000000000, 1.000000000000000000, 1.000000000000000000, 1.000000000000000000, 1.000000000000000000, 1.000000000000000000, 1.000000000000000000, 1.000000000000000000, 1.000000000000000000, 1.000000000000000000, 1.000000000000000000, 1.000000000000000000, 1.000000000000000000, 1.000000000000000000, 1.000000000000000000, 1.000000000000000000, 1.000000000000000000, 1.000000000000000000, 1.000000000000000000, 1.000000000000000000, 1.000000000000000000, 1.000000000000000000, 1.000000000000000000, 1.000000000000000000, 1.000000000000000000, 1.000000000000000000, 1.000000000000000000, 1.000000000000000000, 1.000000000000000000, 1.000000000000000000, 1.000000000000000000, 1.000000000000000000, 1.000000000000000000, 1.000000000000000000, 1.000000000000000000, 1.000000000000000000, 1.000000000000000000, 1.000000000000000000, 1.000000000000000000, 1.000000000000000000, 1.000000000000000000, 1.000000000000000000, 1.000000000000000000, 1.000000000000000000, 1.000000000000000000, 1.000000000000000000, 1.000000000000000000, 1.000000000000000000, 1.000000000000000000, 1.000000000000000000, 1.000000000000000000, 1.000000000000000000, 1.000000000000000000, 1.000000000000000000, 1.000000000000000000, 1.000000000000000000, 1.000000000000000000, 1.000000000000000000, 1.000000000000000000, 1.000000000000000000, 1.000000000000000000, 1.000000000000000000, 1.000000000000000000, 1.000000000000000000, 1.000000000000000000, 1.000000000000000000, 1.000000000000000000, 1.000000000000000000, 1.000000000000000000, 1.000000000000000000, 1.000000000000000000, 1.000000000000000000, 1.000000000000000000, 1.000000000000000000, 1.000000000000000000, 1.000000000000000000, 1.000000000000000000, 1.000000000000000000, 1.000000000000000000, 1.000000000000000000, 1.000000000000000000, 1.000000000000000000, 1.000000000000000000, 1.000000000000000000, 1.000000000000000000, 1.000000000000000000, 1.000000000000000000, 1.000000000000000000, 1.000000000000000000, 1.000000000000000000, 1.000000000000000000, 1.000000000000000000, 1.000000000000000000, 1.000000000000000000, 1.000000000000000000, 1.000000000000000000, 1.000000000000000000, 1.000000000000000000, 1.000000000000000000, 1.000000000000000000, 1.000000000000000000, 1.000000000000000000, 1.000000000000000000, 1.000000000000000000, 1.000000000000000000, 1.000000000000000000, 1.000000000000000000, 1.000000000000000000, 1.000000000000000000, 1.000000000000000000, 1.000000000000000000, 1.000000000000000000, 1.000000000000000000, 1.000000000000000000, 1.000000000000000000, 1.000000000000000000, 1.000000000000000000, 1.000000000000000000, 1.000000000000000000, 1.000000000000000000, 1.000000000000000000, 1.000000000000000000, 1.000000000000000000, 1.000000000000000000, 1.000000000000000000, 1.000000000000000000, 1.000000000000000000, 1.000000000000000000, 1.000000000000000000, 1.000000000000000000, 1.000000000000000000, 1.000000000000000000, 1.000000000000000000, 1.000000000000000000, 1.000000000000000000, 1.000000000000000000, 1.000000000000000000, 1.000000000000000000, 1.000000000000000000, 1.000000000000000000, 1.000000000000000000, 1.000000000000000000, 1.000000000000000000, 1.000000000000000000, 1.000000000000000000, 1.000000000000000000, 1.000000000000000000, 1.000000000000000000, 1.000000000000000000, 1.000000000000000000, 1.000000000000000000, 1.000000000000000000, 1.000000000000000000, 1.000000000000000000, 1.000000000000000000, 1.000000000000000000, 1.000000000000000000, 1.000000000000000000, 1.000000000000000000, 1.000000000000000000, 1.000000000000000000, 1.000000000000000000, 1.000000000000000000, 1.000000000000000000, 1.000000000000000000, 1.000000000000000000, 1.000000000000000000, 1.000000000000000000, 1.000000000000000000, 1.000000000000000000, 1.000000000000000000, 1.000000000000000000, 1.000000000000000000, 1.000000000000000000, 1.000000000000000000, 1.000000000000000000, 1.000000000000000000, 1.000000000000000000, 1.000000000000000000, 1.000000000000000000, 1.000000000000000000, 1.000000000000000000, 1.000000000000000000, 1.000000000000000000, 1.000000000000000000, 1.000000000000000000, 1.000000000000000000, 1.000000000000000000, 1.000000000000000000, 1.000000000000000000, 1.000000000000000000, 1.000000000000000000, 1.000000000000000000, 1.000000000000000000, 1.000000000000000000, 1.000000000000000000, 1.000000000000000000, 1.000000000000000000, 1.000000000000000000, 1.000000000000000000, 1.000000000000000000, 1.000000000000000000, 1.000000000000000000, 1.000000000000000000, 1.000000000000000000, 1.000000000000000000, 1.000000000000000000, 1.000000000000000000, 1.000000000000000000, 1.000000000000000000, 1.000000000000000000, 1.000000000000000000, 1.000000000000000000, 1.000000000000000000, 1.000000000000000000, 1.000000000000000000, 1.000000000000000000, 1.000000000000000000, 1.000000000000000000, 1.000000000000000000, 1.000000000000000000, 1.000000000000000000, 1.000000000000000000, 1.000000000000000000, 1.000000000000000000, 1.000000000000000000, 1.000000000000000000, 1.000000000000000000, 1.000000000000000000, 1.000000000000000000, 1.000000000000000000, 1.000000000000000000, 1.000000000000000000, 1.000000000000000000, 1.000000000000000000, 1.000000000000000000, 1.000000000000000000, 1.000000000000000000, 1.000000000000000000, 1.000000000000000000, 1.000000000000000000, 1.000000000000000000, 1.000000000000000000, 1.000000000000000000, 1.000000000000000000, 1.000000000000000000, 1.000000000000000000, 1.000000000000000000, 1.000000000000000000, 1.000000000000000000, 1.000000000000000000, 1.000000000000000000, 1.000000000000000000, 1.000000000000000000, 1.000000000000000000, 1.000000000000000000, 1.000000000000000000, 1.000000000000000000, 1.000000000000000000, 1.000000000000000000, 1.000000000000000000, 1.000000000000000000, 1.000000000000000000, 1.000000000000000000, 1.000000000000000000, 1.000000000000000000, 1.000000000000000000, 1.000000000000000000, 1.000000000000000000, 1.000000000000000000, 1.000000000000000000, 1.000000000000000000, 1.000000000000000000, 1.000000000000000000, 1.000000000000000000, 1.000000000000000000, 1.000000000000000000, 1.000000000000000000, 1.000000000000000000, 1.000000000000000000, 1.000000000000000000, 1.000000000000000000, 1.000000000000000000, 1.000000000000000000, 1.000000000000000000, 1.000000000000000000, 1.000000000000000000, 1.000000000000000000, 1.000000000000000000, 1.000000000000000000, 1.000000000000000000, 1.000000000000000000, 1.000000000000000000, 1.000000000000000000, 1.000000000000000000, 1.000000000000000000, 1.000000000000000000, 1.000000000000000000, 1.000000000000000000, 1.000000000000000000, 1.000000000000000000, 1.000000000000000000, 1.000000000000000000, 1.000000000000000000, 1.000000000000000000, 1.000000000000000000),
 ( 0.3333333333333333703, 0.3333333333333333703, 0.3333333333333333703, 0.3333333333333333703, 0.3333333333333333703, 0.3333333333333333703, 0.3333333333333333703, 0.3333333333333333703, 0.3333333333333333703, 0.3333333333333333703, 0.3333333333333333703, 0.3333333333333333703, 0.3333333333333333703, 0.3333333333333333703, 0.3333333333333333703, 0.3333333333333333703, 0.3333333333333333703, 0.3333333333333333703, 0.3333333333333333703, 0.3333333333333333703, 0.3333333333333333703, 0.3333333333333333703, 0.3333333333333333703, 0.3333333333333333703, 0.3333333333333333703, 0.3333333333333333703, 0.3333333333333333703, 0.3333333333333333703, 0.3333333333333333703, 0.3333333333333333703, 0.3333333333333333703, 0.3333333333333333703, 0.3333333333333333703, 0.3333333333333333703, 0.3333333333333333703, 0.3333333333333333703, 0.3333333333333333703, 0.3333333333333333703, 0.3333333333333333703, 0.3333333333333333703, 0.3333333333333333703, 0.3333333333333333703, 0.3333333333333333703, 0.3333333333333333703, 0.3333333333333333703, 0.3333333333333333703, 0.3333333333333333703, 0.3333333333333333703, 0.3333333333333333703, 0.3333333333333333703, 0.3333333333333333703, 0.3333333333333333703, 0.3333333333333333703, 0.3333333333333333703, 0.3333333333333333703, 0.3333333333333333703, 0.3333333333333333703, 0.3333333333333333703, 0.3333333333333333703, 0.3333333333333333703, 0.3333333333333333703, 0.3333333333333333703, 0.3333333333333333703, 0.3333333333333333703, 0.3333333333333333703, 0.3333333333333333703, 0.3333333333333333703, 0.3333333333333333703, 0.3333333333333333703, 0.3333333333333333703, 0.3333333333333333703, 0.3333333333333333703, 0.3333333333333333703, 0.3333333333333333703, 0.3333333333333333703, 0.3333333333333333703, 0.3333333333333333703, 0.3333333333333333703, 0.3333333333333333703, 0.3333333333333333703, 0.3333333333333333703, 0.3333333333333333703, 0.3333333333333333703, 0.3333333333333333703, 0.3333333333333333703, 0.3333333333333333703, 0.3333333333333333703, 0.3333333333333333703, 0.3333333333333333703, 0.3333333333333333703, 0.3333333333333333703, 0.3333333333333333703, 0.3333333333333333703, 0.3333333333333333703, 0.3333333333333333703, 0.3333333333333333703, 0.3333333333333333703, 0.3333333333333333703, 0.3333333333333333703, 0.3333333333333333703, 0.3333333333333333703, 0.3333333333333333703, 0.3333333333333333703, 0.3333333333333333703, 0.3333333333333333703, 0.3333333333333333703, 0.3333333333333333703, 0.3333333333333333703, 0.3333333333333333703, 0.3333333333333333703, 0.3333333333333333703, 0.3333333333333333703, 0.3333333333333333703, 0.3333333333333333703, 0.3333333333333333703, 0.3333333333333333703, 0.3333333333333333703, 0.3333333333333333703, 0.3333333333333333703, 0.3333333333333333703, 0.3333333333333333703, 0.3333333333333333703, 0.3333333333333333703, 0.3333333333333333703, 0.3333333333333333703, 0.3333333333333333703, 0.3333333333333333703, 0.3333333333333333703, 0.3333333333333333703, 0.3333333333333333703, 0.3333333333333333703, 0.3333333333333333703, 0.3333333333333333703, 0.3333333333333333703, 0.3333333333333333703, 0.3333333333333333703, 0.3333333333333333703, 0.3333333333333333703, 0.3333333333333333703, 0.3333333333333333703, 0.3333333333333333703, 0.3333333333333333703, 0.3333333333333333703, 0.3333333333333333703, 0.3333333333333333703, 0.3333333333333333703, 0.3333333333333333703, 0.3333333333333333703, 0.3333333333333333703, 0.3333333333333333703, 0.3333333333333333703, 0.3333333333333333703, 0.3333333333333333703, 0.3333333333333333703, 0.3333333333333333703, 0.3333333333333333703, 0.3333333333333333703, 0.3333333333333333703, 0.3333333333333333703, 0.3333333333333333703, 0.3333333333333333703, 0.3333333333333333703, 0.3333333333333333703, 0.3333333333333333703, 0.3333333333333333703, 0.3333333333333333703, 0.3333333333333333703, 0.3333333333333333703, 0.3333333333333333703, 0.3333333333333333703, 0.3333333333333333703, 0.3333333333333333703, 0.3333333333333333703, 0.3333333333333333703, 0.3333333333333333703, 0.3333333333333333703, 0.3333333333333333703, 0.3333333333333333703, 0.3333333333333333703, 0.3333333333333333703, 0.3333333333333333703, 0.3333333333333333703, 0.3333333333333333703, 0.3333333333333333703, 0.3333333333333333703, 0.3333333333333333703, 0.3333333333333333703, 0.3333333333333333703, 0.3333333333333333703, 0.3333333333333333703, 0.3333333333333333703, 0.3333333333333333703, 0.3333333333333333703, 0.3333333333333333703, 0.3333333333333333703, 0.3333333333333333703, 0.3333333333333333703, 0.3333333333333333703, 0.3333333333333333703, 0.3333333333333333703, 0.3333333333333333703, 0.3333333333333333703, 0.3333333333333333703, 0.3333333333333333703, 0.3333333333333333703, 0.3333333333333333703, 0.3333333333333333703, 0.3333333333333333703, 0.3333333333333333703, 0.3333333333333333703, 0.3333333333333333703, 0.3333333333333333703, 0.3333333333333333703, 0.3333333333333333703, 0.3333333333333333703, 0.3333333333333333703, 0.3333333333333333703, 0.3333333333333333703, 0.3333333333333333703, 0.3333333333333333703, 0.3333333333333333703, 0.3333333333333333703, 0.3333333333333333703, 0.3333333333333333703, 0.3333333333333333703, 0.3333333333333333703, 0.3333333333333333703, 0.3333333333333333703, 0.3333333333333333703, 0.3333333333333333703, 0.3333333333333333703, 0.3333333333333333703, 0.3333333333333333703, 0.3333333333333333703, 0.3333333333333333703, 0.3333333333333333703, 0.3333333333333333703, 0.3333333333333333703, 0.3333333333333333703, 0.3333333333333333703, 0.3333333333333333703, 0.3333333333333333703, 0.3333333333333333703, 0.3333333333333333703, 0.3333333333333333703, 0.3333333333333333703, 0.3333333333333333703, 0.3333333333333333703, 0.3333333333333333703, 0.3333333333333333703, 0.3333333333333333703, 0.3333333333333333703, 0.3333333333333333703, 0.3333333333333333703, 0.3333333333333333703, 0.3333333333333333703, 0.3333333333333333703, 0.3333333333333333703, 0.3333333333333333703, 0.3333333333333333703, 0.3333333333333333703, 0.3333333333333333703, 0.3333333333333333703, 0.3333333333333333703, 0.3333333333333333703, 0.3333333333333333703, 0.3333333333333333703, 0.3333333333333333703, 0.3333333333333333703, 0.3333333333333333703, 0.3333333333333333703, 0.3333333333333333703, 0.3333333333333333703, 0.3333333333333333703, 0.3333333333333333703, 0.3333333333333333703, 0.3333333333333333703, 0.3333333333333333703, 0.3333333333333333703, 0.3333333333333333703, 0.3333333333333333703, 0.3333333333333333703, 0.3333333333333333703, 0.3333333333333333703, 0.3333333333333333703, 0.3333333333333333703, 0.3333333333333333703, 0.3333333333333333703, 0.3333333333333333703, 0.3333333333333333703, 0.3333333333333333703, 0.3333333333333333703, 0.3333333333333333703, 0.3333333333333333703, 0.3333333333333333703, 0.3333333333333333703, 0.3333333333333333703, 0.3333333333333333703, 0.3333333333333333703, 0.3333333333333333703, 0.3333333333333333703, 0.3333333333333333703, 0.3333333333333333703, 0.3333333333333333703, 0.3333333333333333703, 0.3333333333333333703, 0.3333333333333333703, 0.3333333333333333703, 0.3333333333333333703, 0.3333333333333333703, 0.3333333333333333703, 0.3333333333333333703, 0.3333333333333333703, 0.3333333333333333703, 0.3333333333333333703, 0.3333333333333333703, 0.3333333333333333703, 0.3333333333333333703, 0.3333333333333333703, 0.3333333333333333703, 0.3333333333333333703, 0.3333333333333333703, 0.3333333333333333703, 0.3333333333333333703, 0.3333333333333333703, 0.3333333333333333703, 0.3333333333333333703, 0.3333333333333333703, 0.3333333333333333703, 0.3333333333333333703, 0.3333333333333333703, 0.3333333333333333703, 0.3333333333333333703, 0.3333333333333333703, 0.3333333333333333703, 0.3333333333333333703),
 ( 0.3333333333333333703, 0.3333333333333333703, 0.3333333333333333703, 0.3333333333333333703, 0.3333333333333333703, 0.3333333333333333703, 0.3333333333333333703, 0.3333333333333333703, 0.3333333333333333703, 0.3333333333333333703, 0.3333333333333333703, 0.3333333333333333703, 0.3333333333333333703, 0.3333333333333333703, 0.3333333333333333703, 0.3333333333333333703, 0.3333333333333333703, 0.3333333333333333703, 0.3333333333333333703, 0.3333333333333333703, 0.3333333333333333703, 0.3333333333333333703, 0.3333333333333333703, 0.3333333333333333703, 0.3333333333333333703, 0.3333333333333333703, 0.3333333333333333703, 0.3333333333333333703, 0.3333333333333333703, 0.3333333333333333703, 0.3333333333333333703, 0.3333333333333333703, 0.3333333333333333703, 0.3333333333333333703, 0.3333333333333333703, 0.3333333333333333703, 0.3333333333333333703, 0.3333333333333333703, 0.3333333333333333703, 0.3333333333333333703, 0.3333333333333333703, 0.3333333333333333703, 0.3333333333333333703, 0.3333333333333333703, 0.3333333333333333703, 0.3333333333333333703, 0.3333333333333333703, 0.3333333333333333703, 0.3333333333333333703, 0.3333333333333333703, 0.3333333333333333703, 0.3333333333333333703, 0.3333333333333333703, 0.3333333333333333703, 0.3333333333333333703, 0.3333333333333333703, 0.3333333333333333703, 0.3333333333333333703, 0.3333333333333333703, 0.3333333333333333703, 0.3333333333333333703, 0.3333333333333333703, 0.3333333333333333703, 0.3333333333333333703, 0.3333333333333333703, 0.3333333333333333703, 0.3333333333333333703, 0.3333333333333333703, 0.3333333333333333703, 0.3333333333333333703, 0.3333333333333333703, 0.3333333333333333703, 0.3333333333333333703, 0.3333333333333333703, 0.3333333333333333703, 0.3333333333333333703, 0.3333333333333333703, 0.3333333333333333703, 0.3333333333333333703, 0.3333333333333333703, 0.3333333333333333703, 0.3333333333333333703, 0.3333333333333333703, 0.3333333333333333703, 0.3333333333333333703, 0.3333333333333333703, 0.3333333333333333703, 0.3333333333333333703, 0.3333333333333333703, 0.3333333333333333703, 0.3333333333333333703, 0.3333333333333333703, 0.3333333333333333703, 0.3333333333333333703, 0.3333333333333333703, 0.3333333333333333703, 0.3333333333333333703, 0.3333333333333333703, 0.3333333333333333703, 0.3333333333333333703, 0.3333333333333333703, 0.3333333333333333703, 0.3333333333333333703, 0.3333333333333333703, 0.3333333333333333703, 0.3333333333333333703, 0.3333333333333333703, 0.3333333333333333703, 0.3333333333333333703, 0.3333333333333333703, 0.3333333333333333703, 0.3333333333333333703, 0.3333333333333333703, 0.3333333333333333703, 0.3333333333333333703, 0.3333333333333333703, 0.3333333333333333703, 0.3333333333333333703, 0.3333333333333333703, 0.3333333333333333703, 0.3333333333333333703, 0.3333333333333333703, 0.3333333333333333703, 0.3333333333333333703, 0.3333333333333333703, 0.3333333333333333703, 0.3333333333333333703, 0.3333333333333333703, 0.3333333333333333703, 0.3333333333333333703, 0.3333333333333333703, 0.3333333333333333703, 0.3333333333333333703, 0.3333333333333333703, 0.3333333333333333703, 0.3333333333333333703, 0.3333333333333333703, 0.3333333333333333703, 0.3333333333333333703, 0.3333333333333333703, 0.3333333333333333703, 0.3333333333333333703, 0.3333333333333333703, 0.3333333333333333703, 0.3333333333333333703, 0.3333333333333333703, 0.3333333333333333703, 0.3333333333333333703, 0.3333333333333333703, 0.3333333333333333703, 0.3333333333333333703, 0.3333333333333333703, 0.3333333333333333703, 0.3333333333333333703, 0.3333333333333333703, 0.3333333333333333703, 0.3333333333333333703, 0.3333333333333333703, 0.3333333333333333703, 0.3333333333333333703, 0.3333333333333333703, 0.3333333333333333703, 0.3333333333333333703, 0.3333333333333333703, 0.3333333333333333703, 0.3333333333333333703, 0.3333333333333333703, 0.3333333333333333703, 0.3333333333333333703, 0.3333333333333333703, 0.3333333333333333703, 0.3333333333333333703, 0.3333333333333333703, 0.3333333333333333703, 0.3333333333333333703, 0.3333333333333333703, 0.3333333333333333703, 0.3333333333333333703, 0.3333333333333333703, 0.3333333333333333703, 0.3333333333333333703, 0.3333333333333333703, 0.3333333333333333703, 0.3333333333333333703, 0.3333333333333333703, 0.3333333333333333703, 0.3333333333333333703, 0.3333333333333333703, 0.3333333333333333703, 0.3333333333333333703, 0.3333333333333333703, 0.3333333333333333703, 0.3333333333333333703, 0.3333333333333333703, 0.3333333333333333703, 0.3333333333333333703, 0.3333333333333333703, 0.3333333333333333703, 0.3333333333333333703, 0.3333333333333333703, 0.3333333333333333703, 0.3333333333333333703, 0.3333333333333333703, 0.3333333333333333703, 0.3333333333333333703, 0.3333333333333333703, 0.3333333333333333703, 0.3333333333333333703, 0.3333333333333333703, 0.3333333333333333703, 0.3333333333333333703, 0.3333333333333333703, 0.3333333333333333703, 0.3333333333333333703, 0.3333333333333333703, 0.3333333333333333703, 0.3333333333333333703, 0.3333333333333333703, 0.3333333333333333703, 0.3333333333333333703, 0.3333333333333333703, 0.3333333333333333703, 0.3333333333333333703, 0.3333333333333333703, 0.3333333333333333703, 0.3333333333333333703, 0.3333333333333333703, 0.3333333333333333703, 0.3333333333333333703, 0.3333333333333333703, 0.3333333333333333703, 0.3333333333333333703, 0.3333333333333333703, 0.3333333333333333703, 0.3333333333333333703, 0.3333333333333333703, 0.3333333333333333703, 0.3333333333333333703, 0.3333333333333333703, 0.3333333333333333703, 0.3333333333333333703, 0.3333333333333333703, 0.3333333333333333703, 0.3333333333333333703, 0.3333333333333333703, 0.3333333333333333703, 0.3333333333333333703, 0.3333333333333333703, 0.3333333333333333703, 0.3333333333333333703, 0.3333333333333333703, 0.3333333333333333703, 0.3333333333333333703, 0.3333333333333333703, 0.3333333333333333703, 0.3333333333333333703, 0.3333333333333333703, 0.3333333333333333703, 0.3333333333333333703, 0.3333333333333333703, 0.3333333333333333703, 0.3333333333333333703, 0.3333333333333333703, 0.3333333333333333703, 0.3333333333333333703, 0.3333333333333333703, 0.3333333333333333703, 0.3333333333333333703, 0.3333333333333333703, 0.3333333333333333703, 0.3333333333333333703, 0.3333333333333333703, 0.3333333333333333703, 0.3333333333333333703, 0.3333333333333333703, 0.3333333333333333703, 0.3333333333333333703, 0.3333333333333333703, 0.3333333333333333703, 0.3333333333333333703, 0.3333333333333333703, 0.3333333333333333703, 0.3333333333333333703, 0.3333333333333333703, 0.3333333333333333703, 0.3333333333333333703, 0.3333333333333333703, 0.3333333333333333703, 0.3333333333333333703, 0.3333333333333333703, 0.3333333333333333703, 0.3333333333333333703, 0.3333333333333333703, 0.3333333333333333703, 0.3333333333333333703, 0.3333333333333333703, 0.3333333333333333703, 0.3333333333333333703, 0.3333333333333333703, 0.3333333333333333703, 0.3333333333333333703, 0.3333333333333333703, 0.3333333333333333703, 0.3333333333333333703, 0.3333333333333333703, 0.3333333333333333703, 0.3333333333333333703, 0.3333333333333333703, 0.3333333333333333703, 0.3333333333333333703, 0.3333333333333333703, 0.3333333333333333703, 0.3333333333333333703, 0.3333333333333333703, 0.3333333333333333703, 0.3333333333333333703, 0.3333333333333333703, 0.3333333333333333703, 0.3333333333333333703, 0.3333333333333333703, 0.3333333333333333703, 0.3333333333333333703, 0.3333333333333333703, 0.3333333333333333703, 0.3333333333333333703, 0.3333333333333333703, 0.3333333333333333703, 0.3333333333333333703, 0.3333333333333333703, 0.3333333333333333703, 0.3333333333333333703, 0.3333333333333333703, 0.3333333333333333703, 0.3333333333333333703, 0.3333333333333333703, 0.3333333333333333703),
 ( 1.000000000000000000, 1.000000000000000000, 1.000000000000000000, 1.000000000000000000, 1.000000000000000000, 1.000000000000000000, 1.000000000000000000, 1.000000000000000000, 1.000000000000000000, 1.000000000000000000, 1.000000000000000000, 1.000000000000000000, 1.000000000000000000, 1.000000000000000000, 1.000000000000000000, 1.000000000000000000, 1.000000000000000000, 1.000000000000000000, 1.000000000000000000, 1.000000000000000000, 1.000000000000000000, 1.000000000000000000, 1.000000000000000000, 1.000000000000000000, 1.000000000000000000, 1.000000000000000000, 1.000000000000000000, 1.000000000000000000, 1.000000000000000000, 1.000000000000000000, 1.000000000000000000, 1.000000000000000000, 1.000000000000000000, 1.000000000000000000, 1.000000000000000000, 1.000000000000000000, 1.000000000000000000, 1.000000000000000000, 1.000000000000000000, 1.000000000000000000, 1.000000000000000000, 1.000000000000000000, 1.000000000000000000, 1.000000000000000000, 1.000000000000000000, 1.000000000000000000, 1.000000000000000000, 1.000000000000000000, 1.000000000000000000, 1.000000000000000000, 1.000000000000000000, 1.000000000000000000, 1.000000000000000000, 1.000000000000000000, 1.000000000000000000, 1.000000000000000000, 1.000000000000000000, 1.000000000000000000, 1.000000000000000000, 1.000000000000000000, 1.000000000000000000, 1.000000000000000000, 1.000000000000000000, 1.000000000000000000, 1.000000000000000000, 1.000000000000000000, 1.000000000000000000, 1.000000000000000000, 1.000000000000000000, 1.000000000000000000, 1.000000000000000000, 1.000000000000000000, 1.000000000000000000, 1.000000000000000000, 1.000000000000000000, 1.000000000000000000, 1.000000000000000000, 1.000000000000000000, 1.000000000000000000, 1.000000000000000000, 1.000000000000000000, 1.000000000000000000, 1.000000000000000000, 1.000000000000000000, 1.000000000000000000, 1.000000000000000000, 1.000000000000000000, 1.000000000000000000, 1.000000000000000000, 1.000000000000000000, 1.000000000000000000, 1.000000000000000000, 1.000000000000000000, 1.000000000000000000, 1.000000000000000000, 1.000000000000000000, 1.000000000000000000, 1.000000000000000000, 1.000000000000000000, 1.000000000000000000, 1.000000000000000000, 1.000000000000000000, 1.000000000000000000, 1.000000000000000000, 1.000000000000000000, 1.000000000000000000, 1.000000000000000000, 1.000000000000000000, 1.000000000000000000, 1.000000000000000000, 1.000000000000000000, 1.000000000000000000, 1.000000000000000000, 1.000000000000000000, 1.000000000000000000, 1.000000000000000000, 1.000000000000000000, 1.000000000000000000, 1.000000000000000000, 1.000000000000000000, 1.000000000000000000, 1.000000000000000000, 1.000000000000000000, 1.000000000000000000, 1.000000000000000000, 1.000000000000000000, 1.000000000000000000, 1.000000000000000000, 1.000000000000000000, 1.000000000000000000, 1.000000000000000000, 1.000000000000000000, 1.000000000000000000, 1.000000000000000000, 1.000000000000000000, 1.000000000000000000, 1.000000000000000000, 1.000000000000000000, 1.000000000000000000, 1.000000000000000000, 1.000000000000000000, 1.000000000000000000, 1.000000000000000000, 1.000000000000000000, 1.000000000000000000, 1.000000000000000000, 1.000000000000000000, 1.000000000000000000, 1.000000000000000000, 1.000000000000000000, 1.000000000000000000, 1.000000000000000000, 1.000000000000000000, 1.000000000000000000, 1.000000000000000000, 1.000000000000000000, 1.000000000000000000, 1.000000000000000000, 1.000000000000000000, 1.000000000000000000, 1.000000000000000000, 1.000000000000000000, 1.000000000000000000, 1.000000000000000000, 1.000000000000000000, 1.000000000000000000, 1.000000000000000000, 1.000000000000000000, 1.000000000000000000, 1.000000000000000000, 1.000000000000000000, 1.000000000000000000, 1.000000000000000000, 1.000000000000000000, 1.000000000000000000, 1.000000000000000000, 1.000000000000000000, 1.000000000000000000, 1.000000000000000000, 1.000000000000000000, 1.000000000000000000, 1.000000000000000000, 1.000000000000000000, 1.000000000000000000, 1.000000000000000000, 1.000000000000000000, 1.000000000000000000, 1.000000000000000000, 1.000000000000000000, 1.000000000000000000, 1.000000000000000000, 1.000000000000000000, 1.000000000000000000, 1.000000000000000000, 1.000000000000000000, 1.000000000000000000, 1.000000000000000000, 1.000000000000000000, 1.000000000000000000, 1.000000000000000000, 1.000000000000000000, 1.000000000000000000, 1.000000000000000000, 1.000000000000000000, 1.000000000000000000, 1.000000000000000000, 1.000000000000000000, 1.000000000000000000, 1.000000000000000000, 1.000000000000000000, 1.000000000000000000, 1.000000000000000000, 1.000000000000000000, 1.000000000000000000, 1.000000000000000000, 1.000000000000000000, 1.000000000000000000, 1.000000000000000000, 1.000000000000000000, 1.000000000000000000, 1.000000000000000000, 1.000000000000000000, 1.000000000000000000, 1.000000000000000000, 1.000000000000000000, 1.000000000000000000, 1.000000000000000000, 1.000000000000000000, 1.000000000000000000, 1.000000000000000000, 1.000000000000000000, 1.000000000000000000, 1.000000000000000000, 1.000000000000000000, 1.000000000000000000, 1.000000000000000000, 1.000000000000000000, 1.000000000000000000, 1.000000000000000000, 1.000000000000000000, 1.000000000000000000, 1.000000000000000000, 1.000000000000000000, 1.000000000000000000, 1.000000000000000000, 1.000000000000000000, 1.000000000000000000, 1.000000000000000000, 1.000000000000000000, 1.000000000000000000, 1.000000000000000000, 1.000000000000000000, 1.000000000000000000, 1.000000000000000000, 1.000000000000000000, 1.000000000000000000, 1.000000000000000000, 1.000000000000000000, 1.000000000000000000, 1.000000000000000000, 1.000000000000000000, 1.000000000000000000, 1.000000000000000000, 1.000000000000000000, 1.000000000000000000, 1.000000000000000000, 1.000000000000000000, 1.000000000000000000, 1.000000000000000000, 1.000000000000000000, 1.000000000000000000, 1.000000000000000000, 1.000000000000000000, 1.000000000000000000, 1.000000000000000000, 1.000000000000000000, 1.000000000000000000, 1.000000000000000000, 1.000000000000000000, 1.000000000000000000, 1.000000000000000000, 1.000000000000000000, 1.000000000000000000, 1.000000000000000000, 1.000000000000000000, 1.000000000000000000, 1.000000000000000000, 1.000000000000000000, 1.000000000000000000, 1.000000000000000000, 1.000000000000000000, 1.000000000000000000, 1.000000000000000000, 1.000000000000000000, 1.000000000000000000, 1.000000000000000000, 1.000000000000000000, 1.000000000000000000, 1.000000000000000000, 1.000000000000000000, 1.000000000000000000, 1.000000000000000000, 1.000000000000000000, 1.000000000000000000, 1.000000000000000000, 1.000000000000000000, 1.000000000000000000, 1.000000000000000000, 1.000000000000000000, 1.000000000000000000, 1.000000000000000000, 1.000000000000000000, 1.000000000000000000, 1.000000000000000000, 1.000000000000000000, 1.000000000000000000, 1.000000000000000000, 1.000000000000000000, 1.000000000000000000, 1.000000000000000000, 1.000000000000000000, 1.000000000000000000, 1.000000000000000000, 1.000000000000000000, 1.000000000000000000, 1.000000000000000000, 1.000000000000000000, 1.000000000000000000, 1.000000000000000000, 1.000000000000000000, 1.000000000000000000, 1.000000000000000000, 1.000000000000000000, 1.000000000000000000, 1.000000000000000000, 1.000000000000000000),
 ( 0.3333333333333333703, 0.3333333333333333703, 0.3333333333333333703, 0.3333333333333333703, 0.3333333333333333703, 0.3333333333333333703, 0.3333333333333333703, 0.3333333333333333703, 0.3333333333333333703, 0.3333333333333333703, 0.3333333333333333703, 0.3333333333333333703, 0.3333333333333333703, 0.3333333333333333703, 0.3333333333333333703, 0.3333333333333333703, 0.3333333333333333703, 0.3333333333333333703, 0.3333333333333333703, 0.3333333333333333703, 0.3333333333333333703, 0.3333333333333333703, 0.3333333333333333703, 0.3333333333333333703, 0.3333333333333333703, 0.3333333333333333703, 0.3333333333333333703, 0.3333333333333333703, 0.3333333333333333703, 0.3333333333333333703, 0.3333333333333333703, 0.3333333333333333703, 0.3333333333333333703, 0.3333333333333333703, 0.3333333333333333703, 0.3333333333333333703, 0.3333333333333333703, 0.3333333333333333703, 0.3333333333333333703, 0.3333333333333333703, 0.3333333333333333703, 0.3333333333333333703, 0.3333333333333333703, 0.3333333333333333703, 0.3333333333333333703, 0.3333333333333333703, 0.3333333333333333703, 0.3333333333333333703, 0.3333333333333333703, 0.3333333333333333703, 0.3333333333333333703, 0.3333333333333333703, 0.3333333333333333703, 0.3333333333333333703, 0.3333333333333333703, 0.3333333333333333703, 0.3333333333333333703, 0.3333333333333333703, 0.3333333333333333703, 0.3333333333333333703, 0.3333333333333333703, 0.3333333333333333703, 0.3333333333333333703, 0.3333333333333333703, 0.3333333333333333703, 0.3333333333333333703, 0.3333333333333333703, 0.3333333333333333703, 0.3333333333333333703, 0.3333333333333333703, 0.3333333333333333703, 0.3333333333333333703, 0.3333333333333333703, 0.3333333333333333703, 0.3333333333333333703, 0.3333333333333333703, 0.3333333333333333703, 0.3333333333333333703, 0.3333333333333333703, 0.3333333333333333703, 0.3333333333333333703, 0.3333333333333333703, 0.3333333333333333703, 0.3333333333333333703, 0.3333333333333333703, 0.3333333333333333703, 0.3333333333333333703, 0.3333333333333333703, 0.3333333333333333703, 0.3333333333333333703, 0.3333333333333333703, 0.3333333333333333703, 0.3333333333333333703, 0.3333333333333333703, 0.3333333333333333703, 0.3333333333333333703, 0.3333333333333333703, 0.3333333333333333703, 0.3333333333333333703, 0.3333333333333333703, 0.3333333333333333703, 0.3333333333333333703, 0.3333333333333333703, 0.3333333333333333703, 0.3333333333333333703, 0.3333333333333333703, 0.3333333333333333703, 0.3333333333333333703, 0.3333333333333333703, 0.3333333333333333703, 0.3333333333333333703, 0.3333333333333333703, 0.3333333333333333703, 0.3333333333333333703, 0.3333333333333333703, 0.3333333333333333703, 0.3333333333333333703, 0.3333333333333333703, 0.3333333333333333703, 0.3333333333333333703, 0.3333333333333333703, 0.3333333333333333703, 0.3333333333333333703, 0.3333333333333333703, 0.3333333333333333703, 0.3333333333333333703, 0.3333333333333333703, 0.3333333333333333703, 0.3333333333333333703, 0.3333333333333333703, 0.3333333333333333703, 0.3333333333333333703, 0.3333333333333333703, 0.3333333333333333703, 0.3333333333333333703, 0.3333333333333333703, 0.3333333333333333703, 0.3333333333333333703, 0.3333333333333333703, 0.3333333333333333703, 0.3333333333333333703, 0.3333333333333333703, 0.3333333333333333703, 0.3333333333333333703, 0.3333333333333333703, 0.3333333333333333703, 0.3333333333333333703, 0.3333333333333333703, 0.3333333333333333703, 0.3333333333333333703, 0.3333333333333333703, 0.3333333333333333703, 0.3333333333333333703, 0.3333333333333333703, 0.3333333333333333703, 0.3333333333333333703, 0.3333333333333333703, 0.3333333333333333703, 0.3333333333333333703, 0.3333333333333333703, 0.3333333333333333703, 0.3333333333333333703, 0.3333333333333333703, 0.3333333333333333703, 0.3333333333333333703, 0.3333333333333333703, 0.3333333333333333703, 0.3333333333333333703, 0.3333333333333333703, 0.3333333333333333703, 0.3333333333333333703, 0.3333333333333333703, 0.3333333333333333703, 0.3333333333333333703, 0.3333333333333333703, 0.3333333333333333703, 0.3333333333333333703, 0.3333333333333333703, 0.3333333333333333703, 0.3333333333333333703, 0.3333333333333333703, 0.3333333333333333703, 0.3333333333333333703, 0.3333333333333333703, 0.3333333333333333703, 0.3333333333333333703, 0.3333333333333333703, 0.3333333333333333703, 0.3333333333333333703, 0.3333333333333333703, 0.3333333333333333703, 0.3333333333333333703, 0.3333333333333333703, 0.3333333333333333703, 0.3333333333333333703, 0.3333333333333333703, 0.3333333333333333703, 0.3333333333333333703, 0.3333333333333333703, 0.3333333333333333703, 0.3333333333333333703, 0.3333333333333333703, 0.3333333333333333703, 0.3333333333333333703, 0.3333333333333333703, 0.3333333333333333703, 0.3333333333333333703, 0.3333333333333333703, 0.3333333333333333703, 0.3333333333333333703, 0.3333333333333333703, 0.3333333333333333703, 0.3333333333333333703, 0.3333333333333333703, 0.3333333333333333703, 0.3333333333333333703, 0.3333333333333333703, 0.3333333333333333703, 0.3333333333333333703, 0.3333333333333333703, 0.3333333333333333703, 0.3333333333333333703, 0.3333333333333333703, 0.3333333333333333703, 0.3333333333333333703, 0.3333333333333333703, 0.3333333333333333703, 0.3333333333333333703, 0.3333333333333333703, 0.3333333333333333703, 0.3333333333333333703, 0.3333333333333333703, 0.3333333333333333703, 0.3333333333333333703, 0.3333333333333333703, 0.3333333333333333703, 0.3333333333333333703, 0.3333333333333333703, 0.3333333333333333703, 0.3333333333333333703, 0.3333333333333333703, 0.3333333333333333703, 0.3333333333333333703, 0.3333333333333333703, 0.3333333333333333703, 0.3333333333333333703, 0.3333333333333333703, 0.3333333333333333703, 0.3333333333333333703, 0.3333333333333333703, 0.3333333333333333703, 0.3333333333333333703, 0.3333333333333333703, 0.3333333333333333703, 0.3333333333333333703, 0.3333333333333333703, 0.3333333333333333703, 0.3333333333333333703, 0.3333333333333333703, 0.3333333333333333703, 0.3333333333333333703, 0.3333333333333333703, 0.3333333333333333703, 0.3333333333333333703, 0.3333333333333333703, 0.3333333333333333703, 0.3333333333333333703, 0.3333333333333333703, 0.3333333333333333703, 0.3333333333333333703, 0.3333333333333333703, 0.3333333333333333703, 0.3333333333333333703, 0.3333333333333333703, 0.3333333333333333703, 0.3333333333333333703, 0.3333333333333333703, 0.3333333333333333703, 0.3333333333333333703, 0.3333333333333333703, 0.3333333333333333703, 0.3333333333333333703, 0.3333333333333333703, 0.3333333333333333703, 0.3333333333333333703, 0.3333333333333333703, 0.3333333333333333703, 0.3333333333333333703, 0.3333333333333333703, 0.3333333333333333703, 0.3333333333333333703, 0.3333333333333333703, 0.3333333333333333703, 0.3333333333333333703, 0.3333333333333333703, 0.3333333333333333703, 0.3333333333333333703, 0.3333333333333333703, 0.3333333333333333703, 0.3333333333333333703, 0.3333333333333333703, 0.3333333333333333703, 0.3333333333333333703, 0.3333333333333333703, 0.3333333333333333703, 0.3333333333333333703, 0.3333333333333333703, 0.3333333333333333703, 0.3333333333333333703, 0.3333333333333333703, 0.3333333333333333703, 0.3333333333333333703, 0.3333333333333333703, 0.3333333333333333703, 0.3333333333333333703, 0.3333333333333333703, 0.3333333333333333703, 0.3333333333333333703, 0.3333333333333333703, 0.3333333333333333703, 0.3333333333333333703, 0.3333333333333333703, 0.3333333333333333703, 0.3333333333333333703, 0.3333333333333333703, 0.3333333333333333703, 0.3333333333333333703, 0.3333333333333333703, 0.3333333333333333703, 0.3333333333333333703, 0.3333333333333333703, 0.3333333333333333703, 0.3333333333333333703, 0.3333333333333333703, 0.3333333333333333703, 0.3333333333333333703),
 ( 0.3333333333333333703, 0.3333333333333333703, 0.3333333333333333703, 0.3333333333333333703, 0.3333333333333333703, 0.3333333333333333703, 0.3333333333333333703, 0.3333333333333333703, 0.3333333333333333703, 0.3333333333333333703, 0.3333333333333333703, 0.3333333333333333703, 0.3333333333333333703, 0.3333333333333333703, 0.3333333333333333703, 0.3333333333333333703, 0.3333333333333333703, 0.3333333333333333703, 0.3333333333333333703, 0.3333333333333333703, 0.3333333333333333703, 0.3333333333333333703, 0.3333333333333333703, 0.3333333333333333703, 0.3333333333333333703, 0.3333333333333333703, 0.3333333333333333703, 0.3333333333333333703, 0.3333333333333333703, 0.3333333333333333703, 0.3333333333333333703, 0.3333333333333333703, 0.3333333333333333703, 0.3333333333333333703, 0.3333333333333333703, 0.3333333333333333703, 0.3333333333333333703, 0.3333333333333333703, 0.3333333333333333703, 0.3333333333333333703, 0.3333333333333333703, 0.3333333333333333703, 0.3333333333333333703, 0.3333333333333333703, 0.3333333333333333703, 0.3333333333333333703, 0.3333333333333333703, 0.3333333333333333703, 0.3333333333333333703, 0.3333333333333333703, 0.3333333333333333703, 0.3333333333333333703, 0.3333333333333333703, 0.3333333333333333703, 0.3333333333333333703, 0.3333333333333333703, 0.3333333333333333703, 0.3333333333333333703, 0.3333333333333333703, 0.3333333333333333703, 0.3333333333333333703, 0.3333333333333333703, 0.3333333333333333703, 0.3333333333333333703, 0.3333333333333333703, 0.3333333333333333703, 0.3333333333333333703, 0.3333333333333333703, 0.3333333333333333703, 0.3333333333333333703, 0.3333333333333333703, 0.3333333333333333703, 0.3333333333333333703, 0.3333333333333333703, 0.3333333333333333703, 0.3333333333333333703, 0.3333333333333333703, 0.3333333333333333703, 0.3333333333333333703, 0.3333333333333333703, 0.3333333333333333703, 0.3333333333333333703, 0.3333333333333333703, 0.3333333333333333703, 0.3333333333333333703, 0.3333333333333333703, 0.3333333333333333703, 0.3333333333333333703, 0.3333333333333333703, 0.3333333333333333703, 0.3333333333333333703, 0.3333333333333333703, 0.3333333333333333703, 0.3333333333333333703, 0.3333333333333333703, 0.3333333333333333703, 0.3333333333333333703, 0.3333333333333333703, 0.3333333333333333703, 0.3333333333333333703, 0.3333333333333333703, 0.3333333333333333703, 0.3333333333333333703, 0.3333333333333333703, 0.3333333333333333703, 0.3333333333333333703, 0.3333333333333333703, 0.3333333333333333703, 0.3333333333333333703, 0.3333333333333333703, 0.3333333333333333703, 0.3333333333333333703, 0.3333333333333333703, 0.3333333333333333703, 0.3333333333333333703, 0.3333333333333333703, 0.3333333333333333703, 0.3333333333333333703, 0.3333333333333333703, 0.3333333333333333703, 0.3333333333333333703, 0.3333333333333333703, 0.3333333333333333703, 0.3333333333333333703, 0.3333333333333333703, 0.3333333333333333703, 0.3333333333333333703, 0.3333333333333333703, 0.3333333333333333703, 0.3333333333333333703, 0.3333333333333333703, 0.3333333333333333703, 0.3333333333333333703, 0.3333333333333333703, 0.3333333333333333703, 0.3333333333333333703, 0.3333333333333333703, 0.3333333333333333703, 0.3333333333333333703, 0.3333333333333333703, 0.3333333333333333703, 0.3333333333333333703, 0.3333333333333333703, 0.3333333333333333703, 0.3333333333333333703, 0.3333333333333333703, 0.3333333333333333703, 0.3333333333333333703, 0.3333333333333333703, 0.3333333333333333703, 0.3333333333333333703, 0.3333333333333333703, 0.3333333333333333703, 0.3333333333333333703, 0.3333333333333333703, 0.3333333333333333703, 0.3333333333333333703, 0.3333333333333333703, 0.3333333333333333703, 0.3333333333333333703, 0.3333333333333333703, 0.3333333333333333703, 0.3333333333333333703, 0.3333333333333333703, 0.3333333333333333703, 0.3333333333333333703, 0.3333333333333333703, 0.3333333333333333703, 0.3333333333333333703, 0.3333333333333333703, 0.3333333333333333703, 0.3333333333333333703, 0.3333333333333333703, 0.3333333333333333703, 0.3333333333333333703, 0.3333333333333333703, 0.3333333333333333703, 0.3333333333333333703, 0.3333333333333333703, 0.3333333333333333703, 0.3333333333333333703, 0.3333333333333333703, 0.3333333333333333703, 0.3333333333333333703, 0.3333333333333333703, 0.3333333333333333703, 0.3333333333333333703, 0.3333333333333333703, 0.3333333333333333703, 0.3333333333333333703, 0.3333333333333333703, 0.3333333333333333703, 0.3333333333333333703, 0.3333333333333333703, 0.3333333333333333703, 0.3333333333333333703, 0.3333333333333333703, 0.3333333333333333703, 0.3333333333333333703, 0.3333333333333333703, 0.3333333333333333703, 0.3333333333333333703, 0.3333333333333333703, 0.3333333333333333703, 0.3333333333333333703, 0.3333333333333333703, 0.3333333333333333703, 0.3333333333333333703, 0.3333333333333333703, 0.3333333333333333703, 0.3333333333333333703, 0.3333333333333333703, 0.3333333333333333703, 0.3333333333333333703, 0.3333333333333333703, 0.3333333333333333703, 0.3333333333333333703, 0.3333333333333333703, 0.3333333333333333703, 0.3333333333333333703, 0.3333333333333333703, 0.3333333333333333703, 0.3333333333333333703, 0.3333333333333333703, 0.3333333333333333703, 0.3333333333333333703, 0.3333333333333333703, 0.3333333333333333703, 0.3333333333333333703, 0.3333333333333333703, 0.3333333333333333703, 0.3333333333333333703, 0.3333333333333333703, 0.3333333333333333703, 0.3333333333333333703, 0.3333333333333333703, 0.3333333333333333703, 0.3333333333333333703, 0.3333333333333333703, 0.3333333333333333703, 0.3333333333333333703, 0.3333333333333333703, 0.3333333333333333703, 0.3333333333333333703, 0.3333333333333333703, 0.3333333333333333703, 0.3333333333333333703, 0.3333333333333333703, 0.3333333333333333703, 0.3333333333333333703, 0.3333333333333333703, 0.3333333333333333703, 0.3333333333333333703, 0.3333333333333333703, 0.3333333333333333703, 0.3333333333333333703, 0.3333333333333333703, 0.3333333333333333703, 0.3333333333333333703, 0.3333333333333333703, 0.3333333333333333703, 0.3333333333333333703, 0.3333333333333333703, 0.3333333333333333703, 0.3333333333333333703, 0.3333333333333333703, 0.3333333333333333703, 0.3333333333333333703, 0.3333333333333333703, 0.3333333333333333703, 0.3333333333333333703, 0.3333333333333333703, 0.3333333333333333703, 0.3333333333333333703, 0.3333333333333333703, 0.3333333333333333703, 0.3333333333333333703, 0.3333333333333333703, 0.3333333333333333703, 0.3333333333333333703, 0.3333333333333333703, 0.3333333333333333703, 0.3333333333333333703, 0.3333333333333333703, 0.3333333333333333703, 0.3333333333333333703, 0.3333333333333333703, 0.3333333333333333703, 0.3333333333333333703, 0.3333333333333333703, 0.3333333333333333703, 0.3333333333333333703, 0.3333333333333333703, 0.3333333333333333703, 0.3333333333333333703, 0.3333333333333333703, 0.3333333333333333703, 0.3333333333333333703, 0.3333333333333333703, 0.3333333333333333703, 0.3333333333333333703, 0.3333333333333333703, 0.3333333333333333703, 0.3333333333333333703, 0.3333333333333333703, 0.3333333333333333703, 0.3333333333333333703, 0.3333333333333333703, 0.3333333333333333703, 0.3333333333333333703, 0.3333333333333333703, 0.3333333333333333703, 0.3333333333333333703, 0.3333333333333333703, 0.3333333333333333703, 0.3333333333333333703, 0.3333333333333333703, 0.3333333333333333703, 0.3333333333333333703, 0.3333333333333333703, 0.3333333333333333703, 0.3333333333333333703, 0.3333333333333333703, 0.3333333333333333703, 0.3333333333333333703, 0.3333333333333333703, 0.3333333333333333703, 0.3333333333333333703, 0.3333333333333333703, 0.3333333333333333703, 0.3333333333333333703, 0.3333333333333333703, 0.3333333333333333703, 0.3333333333333333703, 0.3333333333333333703, 0.3333333333333333703),
 ( 1.000000000000000000, 1.000000000000000000, 1.000000000000000000, 1.000000000000000000, 1.000000000000000000, 1.000000000000000000, 1.000000000000000000, 1.000000000000000000, 1.000000000000000000, 1.000000000000000000, 1.000000000000000000, 1.000000000000000000, 1.000000000000000000, 1.000000000000000000, 1.000000000000000000, 1.000000000000000000, 1.000000000000000000, 1.000000000000000000, 1.000000000000000000, 1.000000000000000000, 1.000000000000000000, 1.000000000000000000, 1.000000000000000000, 1.000000000000000000, 1.000000000000000000, 1.000000000000000000, 1.000000000000000000, 1.000000000000000000, 1.000000000000000000, 1.000000000000000000, 1.000000000000000000, 1.000000000000000000, 1.000000000000000000, 1.000000000000000000, 1.000000000000000000, 1.000000000000000000, 1.000000000000000000, 1.000000000000000000, 1.000000000000000000, 1.000000000000000000, 1.000000000000000000, 1.000000000000000000, 1.000000000000000000, 1.000000000000000000, 1.000000000000000000, 1.000000000000000000, 1.000000000000000000, 1.000000000000000000, 1.000000000000000000, 1.000000000000000000, 1.000000000000000000, 1.000000000000000000, 1.000000000000000000, 1.000000000000000000, 1.000000000000000000, 1.000000000000000000, 1.000000000000000000, 1.000000000000000000, 1.000000000000000000, 1.000000000000000000, 1.000000000000000000, 1.000000000000000000, 1.000000000000000000, 1.000000000000000000, 1.000000000000000000, 1.000000000000000000, 1.000000000000000000, 1.000000000000000000, 1.000000000000000000, 1.000000000000000000, 1.000000000000000000, 1.000000000000000000, 1.000000000000000000, 1.000000000000000000, 1.000000000000000000, 1.000000000000000000, 1.000000000000000000, 1.000000000000000000, 1.000000000000000000, 1.000000000000000000, 1.000000000000000000, 1.000000000000000000, 1.000000000000000000, 1.000000000000000000, 1.000000000000000000, 1.000000000000000000, 1.000000000000000000, 1.000000000000000000, 1.000000000000000000, 1.000000000000000000, 1.000000000000000000, 1.000000000000000000, 1.000000000000000000, 1.000000000000000000, 1.000000000000000000, 1.000000000000000000, 1.000000000000000000, 1.000000000000000000, 1.000000000000000000, 1.000000000000000000, 1.000000000000000000, 1.000000000000000000, 1.000000000000000000, 1.000000000000000000, 1.000000000000000000, 1.000000000000000000, 1.000000000000000000, 1.000000000000000000, 1.000000000000000000, 1.000000000000000000, 1.000000000000000000, 1.000000000000000000, 1.000000000000000000, 1.000000000000000000, 1.000000000000000000, 1.000000000000000000, 1.000000000000000000, 1.000000000000000000, 1.000000000000000000, 1.000000000000000000, 1.000000000000000000, 1.000000000000000000, 1.000000000000000000, 1.000000000000000000, 1.000000000000000000, 1.000000000000000000, 1.000000000000000000, 1.000000000000000000, 1.000000000000000000, 1.000000000000000000, 1.000000000000000000, 1.000000000000000000, 1.000000000000000000, 1.000000000000000000, 1.000000000000000000, 1.000000000000000000, 1.000000000000000000, 1.000000000000000000, 1.000000000000000000, 1.000000000000000000, 1.000000000000000000, 1.000000000000000000, 1.000000000000000000, 1.000000000000000000, 1.000000000000000000, 1.000000000000000000, 1.000000000000000000, 1.000000000000000000, 1.000000000000000000, 1.000000000000000000, 1.000000000000000000, 1.000000000000000000, 1.000000000000000000, 1.000000000000000000, 1.000000000000000000, 1.000000000000000000, 1.000000000000000000, 1.000000000000000000, 1.000000000000000000, 1.000000000000000000, 1.000000000000000000, 1.000000000000000000, 1.000000000000000000, 1.000000000000000000, 1.000000000000000000, 1.000000000000000000, 1.000000000000000000, 1.000000000000000000, 1.000000000000000000, 1.000000000000000000, 1.000000000000000000, 1.000000000000000000, 1.000000000000000000, 1.000000000000000000, 1.000000000000000000, 1.000000000000000000, 1.000000000000000000, 1.000000000000000000, 1.000000000000000000, 1.000000000000000000, 1.000000000000000000, 1.000000000000000000, 1.000000000000000000, 1.000000000000000000, 1.000000000000000000, 1.000000000000000000, 1.000000000000000000, 1.000000000000000000, 1.000000000000000000, 1.000000000000000000, 1.000000000000000000, 1.000000000000000000, 1.000000000000000000, 1.000000000000000000, 1.000000000000000000, 1.000000000000000000, 1.000000000000000000, 1.000000000000000000, 1.000000000000000000, 1.000000000000000000, 1.000000000000000000, 1.000000000000000000, 1.000000000000000000, 1.000000000000000000, 1.000000000000000000, 1.000000000000000000, 1.000000000000000000, 1.000000000000000000, 1.000000000000000000, 1.000000000000000000, 1.000000000000000000, 1.000000000000000000, 1.000000000000000000, 1.000000000000000000, 1.000000000000000000, 1.000000000000000000, 1.000000000000000000, 1.000000000000000000, 1.000000000000000000, 1.000000000000000000, 1.000000000000000000, 1.000000000000000000, 1.000000000000000000, 1.000000000000000000, 1.000000000000000000, 1.000000000000000000, 1.000000000000000000, 1.000000000000000000, 1.000000000000000000, 1.000000000000000000, 1.000000000000000000, 1.000000000000000000, 1.000000000000000000, 1.000000000000000000, 1.000000000000000000, 1.000000000000000000, 1.000000000000000000, 1.000000000000000000, 1.000000000000000000, 1.000000000000000000, 1.000000000000000000, 1.000000000000000000, 1.000000000000000000, 1.000000000000000000, 1.000000000000000000, 1.000000000000000000, 1.000000000000000000, 1.000000000000000000, 1.000000000000000000, 1.000000000000000000, 1.000000000000000000, 1.000000000000000000, 1.000000000000000000, 1.000000000000000000, 1.000000000000000000, 1.000000000000000000, 1.000000000000000000, 1.000000000000000000, 1.000000000000000000, 1.000000000000000000, 1.000000000000000000, 1.000000000000000000, 1.000000000000000000, 1.000000000000000000, 1.000000000000000000, 1.000000000000000000, 1.000000000000000000, 1.000000000000000000, 1.000000000000000000, 1.000000000000000000, 1.000000000000000000, 1.000000000000000000, 1.000000000000000000, 1.000000000000000000, 1.000000000000000000, 1.000000000000000000, 1.000000000000000000, 1.000000000000000000, 1.000000000000000000, 1.000000000000000000, 1.000000000000000000, 1.000000000000000000, 1.000000000000000000, 1.000000000000000000, 1.000000000000000000, 1.000000000000000000, 1.000000000000000000, 1.000000000000000000, 1.000000000000000000, 1.000000000000000000, 1.000000000000000000, 1.000000000000000000, 1.000000000000000000, 1.000000000000000000, 1.000000000000000000, 1.000000000000000000, 1.000000000000000000, 1.000000000000000000, 1.000000000000000000, 1.000000000000000000, 1.000000000000000000, 1.000000000000000000, 1.000000000000000000, 1.000000000000000000, 1.000000000000000000, 1.000000000000000000, 1.000000000000000000, 1.000000000000000000, 1.000000000000000000, 1.000000000000000000, 1.000000000000000000, 1.000000000000000000, 1.000000000000000000, 1.000000000000000000, 1.000000000000000000, 1.000000000000000000, 1.000000000000000000, 1.000000000000000000, 1.000000000000000000, 1.000000000000000000, 1.000000000000000000, 1.000000000000000000, 1.000000000000000000, 1.000000000000000000, 1.000000000000000000, 1.000000000000000000, 1.000000000000000000, 1.000000000000000000, 1.000000000000000000, 1.000000000000000000, 1.000000000000000000, 1.000000000000000000, 1.000000000000000000, 1.000000000000000000, 1.000000000000000000, 1.000000000000000000) ) ) 
 REPRESENTATION_ITEM ( '' )  SURFACE ( )  );
#13780 = AXIS2_PLACEMENT_3D ( 'NONE', #20214, #12214, #1967 ) ;
#13781 = FACE_OUTER_BOUND ( 'NONE', #11665, .T. ) ;
#13782 = CARTESIAN_POINT ( 'NONE',  ( 9.678950682101415737, -24.51930918146190663, -231.5088683414745105 ) ) ;
#13783 = CARTESIAN_POINT ( 'NONE',  ( -10.23029362138610843, 26.44342627367518617, -221.6879936327511871 ) ) ;
#13784 = CARTESIAN_POINT ( 'NONE',  ( 2.485733319737138736, 14.76073968410796056, -221.5245536174130905 ) ) ;
#13785 = CARTESIAN_POINT ( 'NONE',  ( -17.58118739749173898, -8.238107657346720458, -217.5252134542318458 ) ) ;
#13786 = CARTESIAN_POINT ( 'NONE',  ( -15.82036597035495795, 4.920771916499852239, -223.0095317795067160 ) ) ;
#13787 = CARTESIAN_POINT ( 'NONE',  ( 16.11883106748507188, 21.48229216499086291, -233.4985352728212433 ) ) ;
#13788 = ORIENTED_EDGE ( 'NONE', *, *, #4940, .F. ) ;
#13789 = CARTESIAN_POINT ( 'NONE',  ( 10.02513374692848913, 18.81568788741115128, -217.1505009242214612 ) ) ;
#13790 = CARTESIAN_POINT ( 'NONE',  ( 15.22026983281163481, -5.531916908390004828, -229.4891270354009123 ) ) ;
#13791 = CARTESIAN_POINT ( 'NONE',  ( 11.97732832373273126, -6.576952149368169742, -223.6031523087739572 ) ) ;
#13792 = CARTESIAN_POINT ( 'NONE',  ( 0.000000000000000000, 0.000000000000000000, 60.00000000000001421 ) ) ;
#13793 = CARTESIAN_POINT ( 'NONE',  ( 22.84140515590350518, 18.29101041979067332, -226.2334522600520472 ) ) ;
#13794 = CARTESIAN_POINT ( 'NONE',  ( -17.75199675706278413, -2.086992369311378326, -216.9839424855219931 ) ) ;
#13795 = CARTESIAN_POINT ( 'NONE',  ( -7.460068573003235670, -29.58770008691625364, -228.1902472473001637 ) ) ;
#13796 = AXIS2_PLACEMENT_3D ( 'NONE', #8785, #15645, #227 ) ;
#13797 = CARTESIAN_POINT ( 'NONE',  ( 6.131461862964278531, -15.14974102410872625, -231.6805438559109973 ) ) ;
#13798 = AXIS2_PLACEMENT_3D ( 'NONE', #5244, #11795, #12126 ) ;
#13799 = CARTESIAN_POINT ( 'NONE',  ( -3.015877970456246615, 27.27456613555083464, -227.6995284396757313 ) ) ;
#13800 = DIRECTION ( 'NONE',  ( -2.891205793294678696E-17, 0.000000000000000000, -1.000000000000000000 ) ) ;
#13801 = CARTESIAN_POINT ( 'NONE',  ( 12.98277799799954124, 10.30128574332056779, -221.9415428419440559 ) ) ;
#13802 = CARTESIAN_POINT ( 'NONE',  ( -11.98736441306973077, 11.45674391201457176, -217.8252237716743025 ) ) ;
#13803 = CARTESIAN_POINT ( 'NONE',  ( -8.881241380679488984, 27.18697625135247975, -224.4474391433207927 ) ) ;
#13804 = CARTESIAN_POINT ( 'NONE',  ( 13.92699808111095905, -7.117895771238833547, -219.6066573659836081 ) ) ;
#13805 = VERTEX_POINT ( 'NONE', #14928 ) ;
#13806 = CARTESIAN_POINT ( 'NONE',  ( -4.130417896617784912, 16.21758012034559826, -229.8171973319304584 ) ) ;
#13807 = CARTESIAN_POINT ( 'NONE',  ( -23.99493126334580850, 6.052326449358573335, -219.7958990219547672 ) ) ;
#13808 = CARTESIAN_POINT ( 'NONE',  ( 20.82555317450757215, 14.06078233701296476, -215.4201375757437802 ) ) ;
#13809 = CARTESIAN_POINT ( 'NONE',  ( 23.17317677245511831, -6.950782331930943414, -233.5406539459643227 ) ) ;
#13810 = DIRECTION ( 'NONE',  ( 0.000000000000000000, 0.000000000000000000, 1.000000000000000000 ) ) ;
#13811 = VERTEX_POINT ( 'NONE', #6467 ) ;
#13812 = EDGE_CURVE ( 'NONE', #15054, #2965, #20293, .T. ) ;
#13813 = CARTESIAN_POINT ( 'NONE',  ( 0.9908753270255351575, 13.79205759140780430, -228.0165926715089881 ) ) ;
#13814 = CARTESIAN_POINT ( 'NONE',  ( -12.28596215050325924, -1.831058988293407852, -228.6496409048244516 ) ) ;
#13815 = DIRECTION ( 'NONE',  ( -1.000000000000000000, -0.000000000000000000, -0.000000000000000000 ) ) ;
#13816 = CARTESIAN_POINT ( 'NONE',  ( 27.04607490430786854, 4.607450003618843049, -220.3758934308003461 ) ) ;
#13817 = CARTESIAN_POINT ( 'NONE',  ( -15.15434969228324924, 4.423874646950748613, -230.6144467931089821 ) ) ;
#13818 = AXIS2_PLACEMENT_3D ( 'NONE', #5830, #9663, #19882 ) ;
#13819 = CARTESIAN_POINT ( 'NONE',  ( 9.358654279681809740, -11.94480763145079472, -229.8864256833185777 ) ) ;
#13820 = DIRECTION ( 'NONE',  ( -1.000000000000000222, -5.440092820663267048E-15, 0.000000000000000000 ) ) ;
#13821 = CARTESIAN_POINT ( 'NONE',  ( -21.89482327431018760, 1.733733432562314158, -233.1353281693111796 ) ) ;
#13822 = AXIS2_PLACEMENT_3D ( 'NONE', #20178, #18737, #7946 ) ;
#13823 = CARTESIAN_POINT ( 'NONE',  ( -16.20072894238734307, 0.5024448614660336210, -230.4554067149722130 ) ) ;
#13824 = CARTESIAN_POINT ( 'NONE',  ( -5.693514143275418604, -18.22526881224050754, -218.3451910747569968 ) ) ;
#13825 = DIRECTION ( 'NONE',  ( 0.000000000000000000, 1.000000000000000000, -0.000000000000000000 ) ) ;
#13826 = EDGE_CURVE ( 'NONE', #68, #10234, #22075, .T. ) ;
#13827 = DIRECTION ( 'NONE',  ( 0.2588190451025213501, -3.169619151431772337E-17, 0.9659258262890680902 ) ) ;
#13828 = CARTESIAN_POINT ( 'NONE',  ( -27.29953305526601426, 11.21644211419729054, -229.3676346105362995 ) ) ;
#13829 = CARTESIAN_POINT ( 'NONE',  ( 12.37559490515920579, -12.83230305503110991, -219.7713711637379106 ) ) ;
#13830 = CARTESIAN_POINT ( 'NONE',  ( 13.28800886458158104, -2.093462502527361657, -227.1500392263112929 ) ) ;
#13831 = CARTESIAN_POINT ( 'NONE',  ( -23.51643582902884333, 8.486085053562996805, 5.300072969598608630 ) ) ;
#13832 = CARTESIAN_POINT ( 'NONE',  ( 14.12692363916921146, 20.59586666873830296, -230.0804552526094540 ) ) ;
#13833 = CARTESIAN_POINT ( 'NONE',  ( -17.81561310496929806, 18.25637658208611569, -215.7745954696244439 ) ) ;
#13834 = CARTESIAN_POINT ( 'NONE',  ( 12.98277799799954124, 10.30128574332056779, -221.9415428419440559 ) ) ;
#13835 = CARTESIAN_POINT ( 'NONE',  ( -3.542274070161974375, -15.57207032904040389, -222.0010230139451437 ) ) ;
#13836 = CARTESIAN_POINT ( 'NONE',  ( 25.69249634387097814, -4.932549985819596472, -232.9896235759753438 ) ) ;
#13837 = VERTEX_POINT ( 'NONE', #1184 ) ;
#13838 = CARTESIAN_POINT ( 'NONE',  ( -12.62195384480319582, 9.244619650382723819, -228.6283004876635516 ) ) ;
#13839 = CARTESIAN_POINT ( 'NONE',  ( -15.50322565568834321, 9.749075856218723857, -229.6019304695566916 ) ) ;
#13840 = CARTESIAN_POINT ( 'NONE',  ( -12.10258892854866275, 5.599955477755926836, -221.6590149575334010 ) ) ;
#13841 = AXIS2_PLACEMENT_3D ( 'NONE', #21824, #16664, #6414 ) ;
#13842 = CARTESIAN_POINT ( 'NONE',  ( -2.820113134979321590, -27.38213018110698727, -220.3670599055385821 ) ) ;
#13843 = CARTESIAN_POINT ( 'NONE',  ( -0.09137847850202075739, -10.76827681573429807, 92.00000000000000000 ) ) ;
#13844 = EDGE_LOOP ( 'NONE', ( #10367, #1954 ) ) ;
#13845 = CARTESIAN_POINT ( 'NONE',  ( 15.90795275983908574, 2.546196724714939297, -229.0855319561646297 ) ) ;
#13846 = CARTESIAN_POINT ( 'NONE',  ( 10.17740660404977149, -19.92573511251913132, -219.0500883963018737 ) ) ;
#13847 = CARTESIAN_POINT ( 'NONE',  ( 5.017623471397871349, 29.83561274492976878, -222.9769172135417250 ) ) ;
#13848 = CARTESIAN_POINT ( 'NONE',  ( -12.74846050492543625, 19.93509882904884734, -216.0172840992881049 ) ) ;
#13849 = CARTESIAN_POINT ( 'NONE',  ( 12.71499452845021416, 2.172589307656224378, -223.9381607050773084 ) ) ;
#13850 = CARTESIAN_POINT ( 'NONE',  ( 11.67669251569587985, 24.04736029062789981, -218.5856804285192254 ) ) ;
#13851 = DIRECTION ( 'NONE',  ( 0.000000000000000000, 0.000000000000000000, -1.000000000000000000 ) ) ;
#13852 = CIRCLE ( 'NONE', #16017, 2.100000000000000089 ) ;
#13853 = CARTESIAN_POINT ( 'NONE',  ( -6.163092920833200594, -27.00835405423771007, -232.1022292408408987 ) ) ;
#13854 = AXIS2_PLACEMENT_3D ( 'NONE', #15835, #20658, #7175 ) ;
#13855 = CARTESIAN_POINT ( 'NONE',  ( 14.68556740487494849, -6.365102927765655672, -229.6664356779805587 ) ) ;
#13856 = CARTESIAN_POINT ( 'NONE',  ( -19.80000000000007532, 0.000000000000000000, -78.50000000000000000 ) ) ;
#13857 = PLANE ( 'NONE',  #11956 ) ;
#13858 = CARTESIAN_POINT ( 'NONE',  ( 18.06016678184731461, 2.257982981100609354, -218.9983079406065940 ) ) ;
#13859 = CARTESIAN_POINT ( 'NONE',  ( -18.99425472824626482, -3.261482901149847180, -230.2374083206451871 ) ) ;
#13860 = CARTESIAN_POINT ( 'NONE',  ( 30.55431851955342282, 7.682798326916945975, -224.9061577511691610 ) ) ;
#13861 = CARTESIAN_POINT ( 'NONE',  ( 2.508382434586714282, 15.09451298870656011, -220.9010239894319625 ) ) ;
#13862 = CARTESIAN_POINT ( 'NONE',  ( -3.130305314451475418, 18.08417128930788209, -217.9058652980469333 ) ) ;
#13863 = ORIENTED_EDGE ( 'NONE', *, *, #15545, .F. ) ;
#13864 = CARTESIAN_POINT ( 'NONE',  ( 25.14972984070899997, 1.185371537549434029, -234.2576837523010909 ) ) ;
#13865 = CARTESIAN_POINT ( 'NONE',  ( 10.02513374692848913, 18.81568788741115128, -217.1505009242214612 ) ) ;
#13866 = CARTESIAN_POINT ( 'NONE',  ( -19.98042543492610079, 23.51949599776966693, -226.6701036947414138 ) ) ;
#13867 = CARTESIAN_POINT ( 'NONE',  ( -24.19163806436329978, 8.131440952769249719, -230.9341214615949127 ) ) ;
#13868 = CARTESIAN_POINT ( 'NONE',  ( -10.71823000853037655, -10.52987076429259794, -221.3501620068516331 ) ) ;
#13869 = VECTOR ( 'NONE', #15430, 1000.000000000000000 ) ;
#13870 = CIRCLE ( 'NONE', #8834, 2.100000000000000089 ) ;
#13871 = CARTESIAN_POINT ( 'NONE',  ( 0.000000000000000000, 0.000000000000000000, -77.51594804401857175 ) ) ;
#13872 = CARTESIAN_POINT ( 'NONE',  ( 26.91963614581376874, 6.107751173605064920, -232.2246916053503298 ) ) ;
#13873 = CARTESIAN_POINT ( 'NONE',  ( -9.523248388595575875, 12.31121908620753125, -221.6288572946744182 ) ) ;
#13874 = CARTESIAN_POINT ( 'NONE',  ( 5.264801124131998300, 10.54092478143144795, -226.4890466082630098 ) ) ;
#13875 = EDGE_CURVE ( 'NONE', #15721, #4133, #11873, .T. ) ;
#13876 = CARTESIAN_POINT ( 'NONE',  ( -13.92046207272054303, -0.1600067567908077248, -224.5811699126800818 ) ) ;
#13877 = CARTESIAN_POINT ( 'NONE',  ( -30.16874246778906254, -1.865472247480548962, -231.1182156560653880 ) ) ;
#13878 = CARTESIAN_POINT ( 'NONE',  ( -14.84457943406284208, -4.054717634150219574, -219.4128920803699430 ) ) ;
#13879 = CARTESIAN_POINT ( 'NONE',  ( -16.38161496430853248, 17.22219235543852989, -215.3343469598664797 ) ) ;
#13880 = CARTESIAN_POINT ( 'NONE',  ( -5.804961988600464196, -12.67915086496026511, -228.7923277404792088 ) ) ;
#13881 = CARTESIAN_POINT ( 'NONE',  ( -11.26857159993117996, 28.96895336474501192, -225.6039696848669678 ) ) ;
#13882 = CARTESIAN_POINT ( 'NONE',  ( 17.88855223994683286, -5.550763357372503037, -216.0002797835408614 ) ) ;
#13883 = CIRCLE ( 'NONE', #6690, 17.50000000000007816 ) ;
#13884 = CYLINDRICAL_SURFACE ( 'NONE', #13526, 5.500000000000000000 ) ;
#13885 = CIRCLE ( 'NONE', #5964, 25.00000000000010303 ) ;
#13886 = CARTESIAN_POINT ( 'NONE',  ( 24.52160379727246209, 5.049198597839295033, -215.7868787176665535 ) ) ;
#13887 = CARTESIAN_POINT ( 'NONE',  ( -2.100000000000000089, 2.571758278209441957E-16, -105.0000000000000000 ) ) ;
#13888 = CARTESIAN_POINT ( 'NONE',  ( -3.071946796551161984, 23.17078151772539485, -231.0066194318698933 ) ) ;
#13889 = CARTESIAN_POINT ( 'NONE',  ( -18.14952719657095415, 1.368063294522122275, -218.0005379682515922 ) ) ;
#13890 = CARTESIAN_POINT ( 'NONE',  ( 13.69275646168278371, 8.674223198772375909, -220.8699857572541987 ) ) ;
#13891 = CARTESIAN_POINT ( 'NONE',  ( 12.43753614017300713, 2.441361880258234862, -222.2750447601761721 ) ) ;
#13892 = CARTESIAN_POINT ( 'NONE',  ( -0.6614632862528592172, -26.57152937425246719, -233.3304277112415548 ) ) ;
#13893 = CARTESIAN_POINT ( 'NONE',  ( 1.773237071419721422, 13.09828209437875302, -220.6531024550077404 ) ) ;
#13894 = DIRECTION ( 'NONE',  ( 1.000000000000000000, 0.000000000000000000, 0.000000000000000000 ) ) ;
#13895 = CARTESIAN_POINT ( 'NONE',  ( 0.09627406729119250550, -13.23594471221713142, -227.7621942207877339 ) ) ;
#13896 = CARTESIAN_POINT ( 'NONE',  ( -6.720912670637915198, 19.69156892798266512, -217.8848069150180891 ) ) ;
#13897 = VECTOR ( 'NONE', #16668, 1000.000000000000000 ) ;
#13898 = CARTESIAN_POINT ( 'NONE',  ( 13.82984244654956107, 22.51831320572884820, -232.1830460045772213 ) ) ;
#13899 = EDGE_CURVE ( 'NONE', #14126, #15384, #6701, .T. ) ;
#13900 = CARTESIAN_POINT ( 'NONE',  ( -15.89118508636071958, -1.798691612803976492, -229.3605869667087234 ) ) ;
#13901 = CARTESIAN_POINT ( 'NONE',  ( -23.67953786836281083, 9.946055673977088674, -229.5560005648173671 ) ) ;
#13902 = CARTESIAN_POINT ( 'NONE',  ( -19.92987771446595957, 11.92619342620000999, -232.5382020162021206 ) ) ;
#13903 = CARTESIAN_POINT ( 'NONE',  ( 12.91815243135930480, 5.607966342865584153, -224.2227256053222959 ) ) ;
#13904 = ORIENTED_EDGE ( 'NONE', *, *, #10264, .T. ) ;
#13905 = CARTESIAN_POINT ( 'NONE',  ( 4.354034006296288339, 14.09944204372416188, -221.2519525881239417 ) ) ;
#13906 = CARTESIAN_POINT ( 'NONE',  ( 17.04113992636424513, -19.77713422747145700, -220.8032168804961373 ) ) ;
#13907 = CARTESIAN_POINT ( 'NONE',  ( 12.12535264607833341, -6.902938132833007501, -227.3565233277489597 ) ) ;
#13908 = CARTESIAN_POINT ( 'NONE',  ( 0.04449911090679885967, 16.51968908208873899, -222.9067194156212111 ) ) ;
#13909 = AXIS2_PLACEMENT_3D ( 'NONE', #842, #1065, #16379 ) ;
#13910 = ORIENTED_EDGE ( 'NONE', *, *, #4050, .F. ) ;
#13911 = CARTESIAN_POINT ( 'NONE',  ( 12.23063869552301242, 12.84118223717021934, -218.8273164334868284 ) ) ;
#13912 = CARTESIAN_POINT ( 'NONE',  ( -23.43110653090080930, -15.10372739875494297, -233.3642232949313211 ) ) ;
#13913 = CARTESIAN_POINT ( 'NONE',  ( -5.240862053303020573, -11.96147391800445270, -224.1453450823045443 ) ) ;
#13914 = CARTESIAN_POINT ( 'NONE',  ( 1.836136847161299990, -12.84546502099244591, -226.1727064218434293 ) ) ;
#13915 = CARTESIAN_POINT ( 'NONE',  ( -2.532949683519015949, 17.18298404079579100, -229.0924323441805086 ) ) ;
#13916 = DIRECTION ( 'NONE',  ( -1.000000000000000000, 0.000000000000000000, 0.000000000000000000 ) ) ;
#13917 = CARTESIAN_POINT ( 'NONE',  ( 28.46362550855882745, 7.392895870364313282, -223.4682258299149566 ) ) ;
#13918 = CARTESIAN_POINT ( 'NONE',  ( -11.79584727357715934, 6.509288465425584036, -222.6080315736180921 ) ) ;
#13919 = CARTESIAN_POINT ( 'NONE',  ( -8.467651734177735534, 23.23776955534497546, -231.2693664226804913 ) ) ;
#13920 = CARTESIAN_POINT ( 'NONE',  ( -0.9249541874382023465, 14.55235618511626328, -223.7321818898853962 ) ) ;
#13921 = CARTESIAN_POINT ( 'NONE',  ( 14.46993441875745390, 0.2699826811589002284, -230.0986938382904157 ) ) ;
#13922 = CARTESIAN_POINT ( 'NONE',  ( 15.89102655998366664, 24.10108298038447572, -232.7733025413564008 ) ) ;
#13923 = CARTESIAN_POINT ( 'NONE',  ( 7.680972971696337304, -18.49313070787806623, -217.8811398819712508 ) ) ;
#13924 = CARTESIAN_POINT ( 'NONE',  ( 13.72333679673841900, 0.3386527829963648095, -228.4185608440243413 ) ) ;
#13925 = ORIENTED_EDGE ( 'NONE', *, *, #18240, .T. ) ;
#13926 = CARTESIAN_POINT ( 'NONE',  ( -11.42613629117093765, 28.09170287990588832, -228.7150250545069241 ) ) ;
#13927 = CARTESIAN_POINT ( 'NONE',  ( -30.16874246778906254, -1.865472247480548962, -231.1182156560653880 ) ) ;
#13928 = CARTESIAN_POINT ( 'NONE',  ( 27.96460686140487084, -1.872811165202790340, -220.9791906660856000 ) ) ;
#13929 = CARTESIAN_POINT ( 'NONE',  ( 17.99029889091409018, 9.613712288440757092, -232.0298403238024036 ) ) ;
#13930 = CARTESIAN_POINT ( 'NONE',  ( -27.29953305526601426, 11.21644211419729054, -229.3676346105362995 ) ) ;
#13931 = CARTESIAN_POINT ( 'NONE',  ( 15.34510829589250491, -24.56813251781886009, -230.1307231235174982 ) ) ;
#13932 = CARTESIAN_POINT ( 'NONE',  ( 0.000000000000000000, 0.000000000000000000, 0.000000000000000000 ) ) ;
#13933 = CARTESIAN_POINT ( 'NONE',  ( -6.571166997218196748, 12.74865329367398736, -229.9840124400968762 ) ) ;
#13934 = CARTESIAN_POINT ( 'NONE',  ( -26.74045434827795020, 12.41518252455047744, -220.4617428697642652 ) ) ;
#13935 = CARTESIAN_POINT ( 'NONE',  ( -1.198425787605166715, -24.00698511249634137, -218.1862405767648170 ) ) ;
#13936 = LINE ( 'NONE', #15401, #10548 ) ;
#13937 = CARTESIAN_POINT ( 'NONE',  ( 18.54610009393809023, 0.6523581019769808531, -231.1787333216317677 ) ) ;
#13938 = CARTESIAN_POINT ( 'NONE',  ( -21.93900267957129557, 7.862893636934532360, -233.4951761057262161 ) ) ;
#13939 = CARTESIAN_POINT ( 'NONE',  ( 12.89329787743523070, -9.350464391519500040, -225.0861735818250224 ) ) ;
#13941 = ADVANCED_FACE ( 'NONE', ( #16495 ), #3750, .T. ) ;
#13940 = CARTESIAN_POINT ( 'NONE',  ( -29.22168435891936156, -1.352755938724206519, -225.9547066689444250 ) ) ;
#13942 = CARTESIAN_POINT ( 'NONE',  ( -22.91289665287838773, 9.999958348741847303, 0.3307720414079513560 ) ) ;
#13943 = CARTESIAN_POINT ( 'NONE',  ( 21.15841376125116824, 4.865517895153391947, -217.1795922978051578 ) ) ;
#13944 = CARTESIAN_POINT ( 'NONE',  ( -15.42311360645077301, 11.97619046995196079, -234.9244673706848801 ) ) ;
#13945 = CARTESIAN_POINT ( 'NONE',  ( 24.14003655968566520, 13.76285650325712773, -228.1266575292093819 ) ) ;
#13946 = CARTESIAN_POINT ( 'NONE',  ( 4.375292991814291987, -28.67199747747994465, -220.8092881619367631 ) ) ;
#13947 = CARTESIAN_POINT ( 'NONE',  ( 29.08354724566992644, -8.084875104304042992, -220.4391609833976133 ) ) ;
#13948 = EDGE_LOOP ( 'NONE', ( #5955, #3348, #15235, #4380 ) ) ;
#13949 = CARTESIAN_POINT ( 'NONE',  ( 2.508382434586714282, 15.09451298870656011, -220.9010239894319625 ) ) ;
#13950 = CARTESIAN_POINT ( 'NONE',  ( -21.67128887413246119, 15.53484693247673043, -229.0088198863946900 ) ) ;
#13951 = CARTESIAN_POINT ( 'NONE',  ( -11.30246491834384770, 5.534029070539333794, -225.8243940897388597 ) ) ;
#13952 = CARTESIAN_POINT ( 'NONE',  ( -16.95213199947759009, -16.93177456301608785, -219.4409135693619817 ) ) ;
#13953 = CARTESIAN_POINT ( 'NONE',  ( -22.56777165119825668, 2.944661181028116692E-15, 93.00000000000000000 ) ) ;
#13954 = ORIENTED_EDGE ( 'NONE', *, *, #14312, .T. ) ;
#13955 = CARTESIAN_POINT ( 'NONE',  ( 28.09488075336259527, 3.911739131332936381, -227.7543364642411632 ) ) ;
#13956 = CARTESIAN_POINT ( 'NONE',  ( 12.70100985296128115, -15.77027744429350165, -219.4156470604730202 ) ) ;
#13957 = CARTESIAN_POINT ( 'NONE',  ( 14.31308345469695453, 12.76656023072872159, -231.9445021321040770 ) ) ;
#13958 = CARTESIAN_POINT ( 'NONE',  ( -11.49049084071896409, 11.06834963248926940, -218.3354249205727058 ) ) ;
#13959 = CARTESIAN_POINT ( 'NONE',  ( 26.56239871811266440, 9.439457669498057868, -217.7226690415261885 ) ) ;
#13960 = CARTESIAN_POINT ( 'NONE',  ( 15.91295838535984331, 21.88410254487826379, -230.9583961155862823 ) ) ;
#13961 = CARTESIAN_POINT ( 'NONE',  ( -10.76825293233556025, 0.04718088033475291432, 91.99999999999998579 ) ) ;
#13962 = CARTESIAN_POINT ( 'NONE',  ( 1.904360901363437275, -12.77109371939166138, -224.5066922355585177 ) ) ;
#13963 = CARTESIAN_POINT ( 'NONE',  ( 9.918856707546316542, -11.48950767347732871, -219.9734948840342668 ) ) ;
#13964 = CARTESIAN_POINT ( 'NONE',  ( -3.400000000000003908, 3.673940397442062826E-16, -221.9999999999999716 ) ) ;
#13965 = PLANE ( 'NONE',  #12308 ) ;
#13966 = CARTESIAN_POINT ( 'NONE',  ( -13.00859847561873117, 4.399982435993697649, -231.0885370824921097 ) ) ;
#13967 = CARTESIAN_POINT ( 'NONE',  ( -16.80743794350546594, -8.145538706591455735, -220.2004866397506078 ) ) ;
#13968 = CARTESIAN_POINT ( 'NONE',  ( -17.43458823433387650, 2.804998135793385750, -231.8077100320880959 ) ) ;
#13969 = CARTESIAN_POINT ( 'NONE',  ( 3.160467108836292116, 14.95099014189016629, -228.9242958482614370 ) ) ;
#13970 = CARTESIAN_POINT ( 'NONE',  ( 5.711092584709906106, 26.13380667269736790, -220.5232813324456629 ) ) ;
#13971 = ORIENTED_EDGE ( 'NONE', *, *, #18479, .F. ) ;
#13972 = CARTESIAN_POINT ( 'NONE',  ( 16.03771109128167538, -13.01076189404929195, -214.9179096003404084 ) ) ;
#13973 = CARTESIAN_POINT ( 'NONE',  ( 26.29894631880581812, 12.29609390142961090, -226.3100047295820332 ) ) ;
#13974 = CARTESIAN_POINT ( 'NONE',  ( -13.25293905438448405, 17.39325876214774524, -215.6628841494472510 ) ) ;
#13975 = CARTESIAN_POINT ( 'NONE',  ( -23.89856910807799295, 17.42297078648622843, -222.0178620725767757 ) ) ;
#13976 = CARTESIAN_POINT ( 'NONE',  ( -13.66944713747931139, -25.56883467164384527, -222.3908458502962731 ) ) ;
#13977 = EDGE_CURVE ( 'NONE', #21471, #21223, #22114, .T. ) ;
#13978 = DIRECTION ( 'NONE',  ( 1.000000000000000000, 0.000000000000000000, 0.000000000000000000 ) ) ;
#13979 = AXIS2_PLACEMENT_3D ( 'NONE', #2768, #9649, #7744 ) ;
#13980 = DIRECTION ( 'NONE',  ( -0.000000000000000000, -0.000000000000000000, -1.000000000000000000 ) ) ;
#13981 = DIRECTION ( 'NONE',  ( -1.000000000000000000, 0.000000000000000000, 0.000000000000000000 ) ) ;
#13982 = DIRECTION ( 'NONE',  ( -0.000000000000000000, -0.000000000000000000, -1.000000000000000000 ) ) ;
#13983 = CARTESIAN_POINT ( 'NONE',  ( -15.15469129103955304, 15.56563882170958024, -231.6314069158229643 ) ) ;
#13984 = CARTESIAN_POINT ( 'NONE',  ( 20.82555317450757215, 14.06078233701296476, -215.4201375757437802 ) ) ;
#13985 = CARTESIAN_POINT ( 'NONE',  ( -26.02440924314744919, 2.824604386891162111, -232.0644005296583430 ) ) ;
#13986 = CARTESIAN_POINT ( 'NONE',  ( -25.88730550323791491, -2.172607277783750845, -234.4881349215252726 ) ) ;
#13987 = ORIENTED_EDGE ( 'NONE', *, *, #14886, .F. ) ;
#13988 = CARTESIAN_POINT ( 'NONE',  ( -15.34124043857492303, -4.213426711746545372, -218.8308339851419078 ) ) ;
#13989 = AXIS2_PLACEMENT_3D ( 'NONE', #19653, #16404, #14827 ) ;
#13990 = CARTESIAN_POINT ( 'NONE',  ( -7.399925907206128528, 10.29859031525428037, -227.1614041762800298 ) ) ;
#13991 = CARTESIAN_POINT ( 'NONE',  ( -7.531388159411753769, -21.98719092781708540, -216.0713624712111312 ) ) ;
#13992 = CARTESIAN_POINT ( 'NONE',  ( 5.069241901512100412, 14.34986542013820632, -229.6420000777802954 ) ) ;
#13993 = CARTESIAN_POINT ( 'NONE',  ( 9.163585743560105357, -20.90777124155954425, -214.7369711139705259 ) ) ;
#13994 = CARTESIAN_POINT ( 'NONE',  ( -28.42127686227592420, -0.6461176296494712812, -221.6028628238154567 ) ) ;
#13995 = CARTESIAN_POINT ( 'NONE',  ( -16.27882490622757672, 1.520697279646460398, -219.2607721384596289 ) ) ;
#13996 = FACE_OUTER_BOUND ( 'NONE', #9650, .T. ) ;
#13997 = CARTESIAN_POINT ( 'NONE',  ( -2.532949683519015949, 17.18298404079579100, -229.0924323441805086 ) ) ;
#13998 = CARTESIAN_POINT ( 'NONE',  ( 13.98152565379061052, 2.156981915107639036, -230.5667344709999611 ) ) ;
#13999 = CARTESIAN_POINT ( 'NONE',  ( -12.13692969104051400, -0.3108940857385004697, -222.6170402347994184 ) ) ;
#14000 = CARTESIAN_POINT ( 'NONE',  ( 11.83256327006771969, 5.988634687709346593, -225.8999299265561831 ) ) ;
#14001 = CARTESIAN_POINT ( 'NONE',  ( -3.624336683137088677, -15.65024371637965039, -218.6393395577867977 ) ) ;
#14002 = CARTESIAN_POINT ( 'NONE',  ( 9.168912942254459963, 16.03578711007639157, -234.6923200900793347 ) ) ;
#14003 = CARTESIAN_POINT ( 'NONE',  ( 16.07305932912010960, 0.9253679043337685872, -229.0409936706996064 ) ) ;
#14004 = CARTESIAN_POINT ( 'NONE',  ( -14.99584720478923572, -27.01727836854440312, -219.7524089968786996 ) ) ;
#14005 = CARTESIAN_POINT ( 'NONE',  ( -4.490213599459100813, 14.55066867058898694, -222.6488251579668827 ) ) ;
#14006 = CARTESIAN_POINT ( 'NONE',  ( 10.70175380652492336, 7.370128018021000038, -224.3479584370086286 ) ) ;
#14007 = CARTESIAN_POINT ( 'NONE',  ( -14.73155177304599306, -1.817590056890399763, -226.9769936995019748 ) ) ;
#14008 = CARTESIAN_POINT ( 'NONE',  ( -15.37153448429513602, 5.014568651886798456, -224.5085656291724945 ) ) ;
#14009 = CARTESIAN_POINT ( 'NONE',  ( -4.531689447889125866, 14.11317536318881416, -231.6806015375303502 ) ) ;
#14010 = CARTESIAN_POINT ( 'NONE',  ( 16.10828274231666768, 3.530956590605524692, -220.6574330336208050 ) ) ;
#14011 = ORIENTED_EDGE ( 'NONE', *, *, #12242, .F. ) ;
#14012 = CARTESIAN_POINT ( 'NONE',  ( 7.764422566766373990, -15.81008911711046672, -220.9836405809557220 ) ) ;
#14013 = VERTEX_POINT ( 'NONE', #8396 ) ;
#14014 = CARTESIAN_POINT ( 'NONE',  ( 5.133806223762193532, -16.42362916962670383, -230.4968203642818310 ) ) ;
#14015 = CARTESIAN_POINT ( 'NONE',  ( -2.906906946766868227, 27.66682465340607422, -226.6559963821499082 ) ) ;
#14016 = PRODUCT_DEFINITION ( 'UNKNOWN', '', #939, #656 ) ;
#14017 = DIRECTION ( 'NONE',  ( -1.083936797661035110E-15, -1.000000000000000000, 0.000000000000000000 ) ) ;
#14018 = CARTESIAN_POINT ( 'NONE',  ( 13.69275646168278371, 8.674223198772375909, -220.8699857572541987 ) ) ;
#14019 = CARTESIAN_POINT ( 'NONE',  ( 28.22932473237819551, -8.039268142081398949, -226.6539694142420558 ) ) ;
#14020 = CARTESIAN_POINT ( 'NONE',  ( -16.39524763169126942, -10.97410814576847926, -232.9630882351523837 ) ) ;
#14021 = CARTESIAN_POINT ( 'NONE',  ( 1.127544764349826867, -27.89617517048659323, -231.9509945439240823 ) ) ;
#14022 = CARTESIAN_POINT ( 'NONE',  ( -5.764806379010653181, 14.19340719117484007, -223.8851086052821415 ) ) ;
#14023 = DIRECTION ( 'NONE',  ( 1.000000000000000000, 0.000000000000000000, 0.000000000000000000 ) ) ;
#14024 = CARTESIAN_POINT ( 'NONE',  ( 19.67070349224072956, 16.44307963282299312, -220.0378483479504439 ) ) ;
#14025 = CARTESIAN_POINT ( 'NONE',  ( -15.66530208164916260, 23.23467148471576849, -218.1250122661128046 ) ) ;
#14026 = CARTESIAN_POINT ( 'NONE',  ( -10.94147694953847250, 13.90730769817462864, -218.7797619932150042 ) ) ;
#14027 = VERTEX_POINT ( 'NONE', #8278 ) ;
#14028 = CARTESIAN_POINT ( 'NONE',  ( 7.772443558932104146, 25.24620711463332157, -231.7813173736589931 ) ) ;
#14029 = CARTESIAN_POINT ( 'NONE',  ( -27.28038240442402440, 5.683827137705129040, -226.0726697751923382 ) ) ;
#14030 = CARTESIAN_POINT ( 'NONE',  ( 13.49694890958685711, 2.186465430673721677, -228.8273158381700512 ) ) ;
#14031 = CARTESIAN_POINT ( 'NONE',  ( 19.66153801111809685, -22.47763448259700780, -224.4992982350615023 ) ) ;
#14032 = DIRECTION ( 'NONE',  ( -1.000000000000000000, 1.224646799147351482E-16, 0.000000000000000000 ) ) ;
#14033 = EDGE_LOOP ( 'NONE', ( #10704, #276, #12319, #15281 ) ) ;
#14034 = CARTESIAN_POINT ( 'NONE',  ( -6.201839134465864767, 11.37481922992157379, -223.7040893475979146 ) ) ;
#14035 = CARTESIAN_POINT ( 'NONE',  ( 27.35305420947085153, -2.513179086165481912, -228.1718430395816881 ) ) ;
#14036 = LINE ( 'NONE', #8860, #16562 ) ;
#14037 = CARTESIAN_POINT ( 'NONE',  ( 22.18132842682159733, 5.591149267797686839, -232.0584733989884114 ) ) ;
#14038 = CARTESIAN_POINT ( 'NONE',  ( -13.92046207272054303, -0.1600067567908077248, -224.5811699126800818 ) ) ;
#14039 = CARTESIAN_POINT ( 'NONE',  ( 7.080148886126969465, -28.65852557119563926, -219.9679292432588227 ) ) ;
#14040 = DIRECTION ( 'NONE',  ( 1.000000000000000000, 0.000000000000000000, 0.000000000000000000 ) ) ;
#14041 = CARTESIAN_POINT ( 'NONE',  ( -8.501641725227710111, 25.47064987787527102, -217.3358698761548737 ) ) ;
#14042 = CARTESIAN_POINT ( 'NONE',  ( -12.26337789213896201, 9.274758280606999250, -219.9806108963443876 ) ) ;
#14043 = VERTEX_POINT ( 'NONE', #11429 ) ;
#14044 = CARTESIAN_POINT ( 'NONE',  ( -16.63766460830045091, 5.158675778507696208, -232.1659425527909093 ) ) ;
#14045 = CARTESIAN_POINT ( 'NONE',  ( -10.30161254035895091, -9.966167094494833734, -223.3409979381218875 ) ) ;
#14046 = PLANE ( 'NONE',  #11633 ) ;
#14047 = DIRECTION ( 'NONE',  ( 0.000000000000000000, 0.000000000000000000, -1.000000000000000000 ) ) ;
#14048 = CARTESIAN_POINT ( 'NONE',  ( -27.82842955277035202, 11.70195273568964112, -227.9294339757464911 ) ) ;
#14049 = CARTESIAN_POINT ( 'NONE',  ( 3.737366178615106893, -15.16223317163647621, -230.3303395318446292 ) ) ;
#14050 =( NAMED_UNIT ( * ) SI_UNIT ( $, .STERADIAN. ) SOLID_ANGLE_UNIT ( ) );
#14051 = DIRECTION ( 'NONE',  ( 1.000000000000000000, 0.000000000000000000, 0.000000000000000000 ) ) ;
#14052 = CARTESIAN_POINT ( 'NONE',  ( 20.90058474538433231, 18.60939544422136294, -225.8027644507526475 ) ) ;
#14053 = CARTESIAN_POINT ( 'NONE',  ( -16.96626096607909417, 26.06638125783293347, -227.3272535207661349 ) ) ;
#14054 = LINE ( 'NONE', #10140, #1307 ) ;
#14055 = CARTESIAN_POINT ( 'NONE',  ( 15.54095364727189299, 10.52000078266145700, -230.2714373371992735 ) ) ;
#14056 = CARTESIAN_POINT ( 'NONE',  ( -2.278185930139247084, -29.13041568434719863, -223.8160414879089046 ) ) ;
#14057 = CARTESIAN_POINT ( 'NONE',  ( 13.45252989138277400, -0.3779036657139918098, -224.7462000225944792 ) ) ;
#14058 = ORIENTED_EDGE ( 'NONE', *, *, #9702, .F. ) ;
#14059 = APPLICATION_CONTEXT ( 'automotive_design' ) ;
#14060 = CARTESIAN_POINT ( 'NONE',  ( 1.656472371294090085, 27.29382523973669095, -230.4991099578876117 ) ) ;
#14061 = CARTESIAN_POINT ( 'NONE',  ( -16.88145396433676027, 5.002512658926777434, -221.2364783498041731 ) ) ;
#14062 = CARTESIAN_POINT ( 'NONE',  ( -23.49520248890869212, 11.82830312093803649, -233.3871405502527807 ) ) ;
#14063 = CARTESIAN_POINT ( 'NONE',  ( -14.19990609618026056, -7.901335420714983293, -227.4892254059333823 ) ) ;
#14064 = DIRECTION ( 'NONE',  ( -0.000000000000000000, -0.000000000000000000, 1.000000000000000000 ) ) ;
#14065 = ORIENTED_EDGE ( 'NONE', *, *, #16549, .F. ) ;
#14066 = CARTESIAN_POINT ( 'NONE',  ( 27.16757474806794903, 2.676291341565463888, -220.8863403533574115 ) ) ;
#14067 = CARTESIAN_POINT ( 'NONE',  ( -2.821634405314548566, -24.60373223977012458, -232.0829149086248435 ) ) ;
#14068 = CARTESIAN_POINT ( 'NONE',  ( 13.43730899468209294, 8.427513769504761498, -221.4030804848920297 ) ) ;
#14069 = CARTESIAN_POINT ( 'NONE',  ( -9.740348021262962064, 16.12529029871877384, -216.4361617420699702 ) ) ;
#14070 = EDGE_CURVE ( 'NONE', #19932, #14271, #4474, .T. ) ;
#14071 = CARTESIAN_POINT ( 'NONE',  ( 27.08260752785270853, 4.114838227474355570, -232.2882281786467331 ) ) ;
#14072 = CARTESIAN_POINT ( 'NONE',  ( 5.623554730548537606, 15.65270319720736225, -231.3185741195121068 ) ) ;
#14073 = CYLINDRICAL_SURFACE ( 'NONE', #8042, 2.000000000000000000 ) ;
#14074 = CARTESIAN_POINT ( 'NONE',  ( -8.257247207528708444, -26.39349301559143512, -217.9383130379005138 ) ) ;
#14075 = CARTESIAN_POINT ( 'NONE',  ( 20.98776729843937972, -13.55153944770713359, -217.5092423276211946 ) ) ;
#14076 = FACE_OUTER_BOUND ( 'NONE', #2500, .T. ) ;
#14077 = FACE_OUTER_BOUND ( 'NONE', #9756, .T. ) ;
#14078 = CARTESIAN_POINT ( 'NONE',  ( -13.91932826323387395, 8.983986115891950064, -216.4624824187541776 ) ) ;
#14079 = CARTESIAN_POINT ( 'NONE',  ( 23.66932040738428356, 1.377632087272899541, -234.6098499860491415 ) ) ;
#14080 = CARTESIAN_POINT ( 'NONE',  ( 21.17011458613547248, 1.652544727609948527, -234.6098499860487152 ) ) ;
#14081 = CARTESIAN_POINT ( 'NONE',  ( 1.939863782649466017, 28.20584428268631783, -229.4487744520996273 ) ) ;
#14082 = CARTESIAN_POINT ( 'NONE',  ( 5.248013545904832711, 18.51731616863089158, -219.3673127389703552 ) ) ;
#14083 = ORIENTED_EDGE ( 'NONE', *, *, #6929, .F. ) ;
#14084 = CARTESIAN_POINT ( 'NONE',  ( 13.86864723624500328, -7.301706307425273046, -233.2436966314882909 ) ) ;
#14085 = ORIENTED_EDGE ( 'NONE', *, *, #11000, .T. ) ;
#14086 = CARTESIAN_POINT ( 'NONE',  ( 24.03642272140365677, 3.646960756862087205, -218.2320643939070806 ) ) ;
#14087 = CARTESIAN_POINT ( 'NONE',  ( -17.20794623181132721, 21.97849129791581291, -217.9187454682870850 ) ) ;
#14088 = CARTESIAN_POINT ( 'NONE',  ( -16.88427011841620029, 9.219900108593305887, -231.9155403335099948 ) ) ;
#14089 = CARTESIAN_POINT ( 'NONE',  ( -15.33992272861872763, -7.600289318192222865, -231.6130094852651951 ) ) ;
#14090 = CARTESIAN_POINT ( 'NONE',  ( -11.46843428684449151, 6.508406145394057596, -225.7212143570321814 ) ) ;
#14091 = DIRECTION ( 'NONE',  ( 0.000000000000000000, 0.000000000000000000, -1.000000000000000000 ) ) ;
#14092 = EDGE_CURVE ( 'NONE', #11155, #15054, #18846, .T. ) ;
#14093 = DIRECTION ( 'NONE',  ( -1.000000000000000000, 0.000000000000000000, 0.000000000000000000 ) ) ;
#14094 = CARTESIAN_POINT ( 'NONE',  ( 12.88374853655145458, 4.106359831454843068, -228.1016120772327440 ) ) ;
#14095 = VECTOR ( 'NONE', #18126, 1000.000000000000000 ) ;
#14096 = CARTESIAN_POINT ( 'NONE',  ( -13.41250421226414069, 17.27419134292087577, -217.6844171132545966 ) ) ;
#14097 = CARTESIAN_POINT ( 'NONE',  ( 15.79748369401691122, 19.19631269170049137, -215.0096632418193963 ) ) ;
#14098 = CARTESIAN_POINT ( 'NONE',  ( -13.10651848559790444, 3.262242204071156948, -224.3513854875720597 ) ) ;
#14099 = CARTESIAN_POINT ( 'NONE',  ( -22.78031074599627814, -9.151179398885634697, -235.0532497368941733 ) ) ;
#14100 = AXIS2_PLACEMENT_3D ( 'NONE', #18540, #20429, #17184 ) ;
#14101 = CARTESIAN_POINT ( 'NONE',  ( -19.18273340400098448, -14.85130345181434741, -232.7114379411565039 ) ) ;
#14102 = EDGE_CURVE ( 'NONE', #1959, #3502, #12030, .T. ) ;
#14103 = CARTESIAN_POINT ( 'NONE',  ( -12.38801939673351704, 9.361418580567464787, -232.8075769614211765 ) ) ;
#14104 = CARTESIAN_POINT ( 'NONE',  ( -8.258403559667634397, -29.80786866836635696, -223.3983869762195127 ) ) ;
#14105 = CARTESIAN_POINT ( 'NONE',  ( 4.354034006296288339, 14.09944204372416188, -221.2519525881239417 ) ) ;
#14106 = CARTESIAN_POINT ( 'NONE',  ( 11.14866046433140490, -17.10865642060806024, -235.2771047445726822 ) ) ;
#14107 = CARTESIAN_POINT ( 'NONE',  ( -27.09167109716269550, -0.2825935922571593539, -219.8389404328913486 ) ) ;
#14108 = CARTESIAN_POINT ( 'NONE',  ( -18.04772061096520375, 5.916925414182395038, -217.8829197293425750 ) ) ;
#14109 = FILL_AREA_STYLE_COLOUR ( '', #6692 ) ;
#14110 = CARTESIAN_POINT ( 'NONE',  ( -9.106229537879125147, 25.89784491087598184, -228.9807674929363372 ) ) ;
#14111 = CARTESIAN_POINT ( 'NONE',  ( -28.31595744342370580, 5.786754998807587924, -229.0820962600229223 ) ) ;
#14112 = AXIS2_PLACEMENT_3D ( 'NONE', #16432, #6172, #6399 ) ;
#14113 = CARTESIAN_POINT ( 'NONE',  ( 26.29894631880581812, 12.29609390142961090, -226.3100047295820332 ) ) ;
#14114 = CARTESIAN_POINT ( 'NONE',  ( 14.55590852435181226, 2.816890518231522034, -218.5131513550309990 ) ) ;
#14115 = CARTESIAN_POINT ( 'NONE',  ( -15.44264673875841432, -21.96030778071044054, -219.6531968376115174 ) ) ;
#14116 = ADVANCED_FACE ( 'NONE', ( #19286 ), #10187, .F. ) ;
#14117 = CARTESIAN_POINT ( 'NONE',  ( 6.550054208186137039, 12.38618022562281595, -231.5087189857719068 ) ) ;
#14118 = CARTESIAN_POINT ( 'NONE',  ( 25.50000000000000000, 0.000000000000000000, 0.000000000000000000 ) ) ;
#14119 = CARTESIAN_POINT ( 'NONE',  ( -13.66010072360327676, -23.28416639572314750, -215.9262288161416166 ) ) ;
#14120 = CARTESIAN_POINT ( 'NONE',  ( -4.080659539198054020, 15.43130099126780408, -228.8058965243247656 ) ) ;
#14121 = CARTESIAN_POINT ( 'NONE',  ( 8.554868430186942874, 10.42313681336814568, -223.0114508542762621 ) ) ;
#14122 = VECTOR ( 'NONE', #2349, 1000.000000000000000 ) ;
#14123 = CARTESIAN_POINT ( 'NONE',  ( -15.82068653568960137, 8.372322471091806051, -220.7139663195713979 ) ) ;
#14124 = CARTESIAN_POINT ( 'NONE',  ( -0.04850409037381671340, 14.20520396026658716, -231.8092226852533031 ) ) ;
#14125 = CARTESIAN_POINT ( 'NONE',  ( 24.78377098693636427, 3.871650763546384155, -231.3521132786341923 ) ) ;
#14126 = VERTEX_POINT ( 'NONE', #20969 ) ;
#14127 = CARTESIAN_POINT ( 'NONE',  ( 13.12950778469841318, -23.99547238938880511, -222.5250877844293029 ) ) ;
#14128 = EDGE_LOOP ( 'NONE', ( #976, #8251, #13525, #7167 ) ) ;
#14129 = CARTESIAN_POINT ( 'NONE',  ( 19.57710422433000019, -21.48596639614413562, -228.6055549924913635 ) ) ;
#14130 = CARTESIAN_POINT ( 'NONE',  ( -2.554014161526931392, 17.56271496069470572, -229.4905841158208659 ) ) ;
#14131 = FILL_AREA_STYLE_COLOUR ( '', #3386 ) ;
#14132 = CARTESIAN_POINT ( 'NONE',  ( 22.02796522526679723, 16.41909032291435366, -220.1590600991317217 ) ) ;
#14133 = CARTESIAN_POINT ( 'NONE',  ( -30.56371166594826150, 0.09613004385584933420, -226.3268674980304525 ) ) ;
#14134 = CARTESIAN_POINT ( 'NONE',  ( -21.52428768452188734, -21.65989873160339840, -225.4304055049964006 ) ) ;
#14135 = CARTESIAN_POINT ( 'NONE',  ( 6.589392574981438599, -17.08498810221841069, -232.9613445306918322 ) ) ;
#14136 = CARTESIAN_POINT ( 'NONE',  ( -8.881241380679488984, 27.18697625135247975, -224.4474391433207927 ) ) ;
#14137 = CARTESIAN_POINT ( 'NONE',  ( -10.76794919243112325, 0.000000000000000000, 93.00000000000000000 ) ) ;
#14138 = CARTESIAN_POINT ( 'NONE',  ( 20.59763700141659015, 7.383112456150029423, -232.0722244125682039 ) ) ;
#14139 = CARTESIAN_POINT ( 'NONE',  ( -9.540790481621398200, 9.981116473660406996, -228.6478862620407995 ) ) ;
#14140 = CARTESIAN_POINT ( 'NONE',  ( -3.926352947695993745, 17.69140300707508473, -220.1607884481205986 ) ) ;
#14141 = EDGE_LOOP ( 'NONE', ( #8632, #7835 ) ) ;
#14142 = AXIS2_PLACEMENT_3D ( 'NONE', #2324, #9093, #9209 ) ;
#14143 = AXIS2_PLACEMENT_3D ( 'NONE', #6619, #13800, #13916 ) ;
#14144 = CARTESIAN_POINT ( 'NONE',  ( 7.450672702945051462, 17.42371045663376705, -217.2894981592719432 ) ) ;
#14145 = CARTESIAN_POINT ( 'NONE',  ( -18.94009481283715957, 3.115208415279245191, -230.3622730452590588 ) ) ;
#14146 = CARTESIAN_POINT ( 'NONE',  ( 13.70863938672594529, 6.616599615120571265, -232.1343637516268643 ) ) ;
#14147 = CARTESIAN_POINT ( 'NONE',  ( 12.20621255000322947, -21.57429421806300240, -232.1397031738524674 ) ) ;
#14148 = CARTESIAN_POINT ( 'NONE',  ( 18.40125535140034430, 0.01434342441762339639, -233.2485400239426099 ) ) ;
#14149 = ORIENTED_EDGE ( 'NONE', *, *, #3156, .T. ) ;
#14150 = CARTESIAN_POINT ( 'NONE',  ( 7.769483725421269860, 20.68783433326350263, -233.2348178266662728 ) ) ;
#14151 = CARTESIAN_POINT ( 'NONE',  ( 22.49864633775863609, -6.670857247392108391, -230.7634588385486438 ) ) ;
#14152 = CARTESIAN_POINT ( 'NONE',  ( 0.000000000000000000, 20.99999999999999645, 69.99999999999998579 ) ) ;
#14153 = CARTESIAN_POINT ( 'NONE',  ( 14.80394259695730064, 1.224172658189580432, -225.4564070658925061 ) ) ;
#14154 = CARTESIAN_POINT ( 'NONE',  ( 1.799766247726228174, -14.75051420185460849, -230.6199496058247291 ) ) ;
#14155 = B_SPLINE_CURVE_WITH_KNOTS ( 'NONE', 3,
 ( #13604, #20328, #3004, #22147, #18667, #9887, #16753, #10110, #20441, #5030, #18771, #3339, #17090, #15508, #3669, #21002, #20776, #3788, #12473, #12357, #19207, #89 ),
 .UNSPECIFIED., .F., .F.,
 ( 4, 2, 2, 2, 2, 2, 2, 2, 2, 2, 4 ),
 ( -1.095445575531460033E-05, 0.0003522495710957299596, 0.0007154535979467744602, 0.001441861651648853378, 0.002168269705350933489, 0.002894677759053012733, 0.003621085812755091976, 0.004347493866457172521, 0.005073901920159251330, 0.005437105947010329766, 0.005800309973861407335 ),
 .UNSPECIFIED. ) ;
#14156 = CARTESIAN_POINT ( 'NONE',  ( -18.39892766464214446, 25.11039525536027739, -225.3444503920457294 ) ) ;
#14158 = CARTESIAN_POINT ( 'NONE',  ( -9.251743101293765648, 14.06372330290396278, -232.4239003576353468 ) ) ;
#14157 = AXIS2_PLACEMENT_3D ( 'NONE', #6045, #18099, #2448 ) ;
#14159 = ORIENTED_EDGE ( 'NONE', *, *, #13899, .T. ) ;
#14160 = CARTESIAN_POINT ( 'NONE',  ( -15.82069055112642353, 8.315535108674763976, -217.2800172218543935 ) ) ;
#14161 = CARTESIAN_POINT ( 'NONE',  ( -14.31049420963804586, -8.435107166214018903, -218.7432863707801403 ) ) ;
#14162 = CIRCLE ( 'NONE', #4778, 17.50000000000000711 ) ;
#14163 = DIRECTION ( 'NONE',  ( -1.000000000000000000, 0.000000000000000000, 0.000000000000000000 ) ) ;
#14164 = CARTESIAN_POINT ( 'NONE',  ( 0.000000000000000000, 23.00000000000006395, -75.00000000000000000 ) ) ;
#14165 = CARTESIAN_POINT ( 'NONE',  ( -14.68037037322036475, 3.441677802729143920, -220.1396515630443389 ) ) ;
#14166 = CARTESIAN_POINT ( 'NONE',  ( 6.028509222145709501, -20.27756025184508815, -216.6192952284833950 ) ) ;
#14167 = CARTESIAN_POINT ( 'NONE',  ( 25.50000000000000000, 4.399999999999999467, -3.300000000000000266 ) ) ;
#14168 = CARTESIAN_POINT ( 'NONE',  ( 25.53003411612920459, 7.940385729200389875, -230.5495695598654322 ) ) ;
#14169 = CARTESIAN_POINT ( 'NONE',  ( -15.64710113362562183, 25.90300453978063189, -220.8637308366217269 ) ) ;
#14170 = CARTESIAN_POINT ( 'NONE',  ( -1.232595164407830946E-29, 17.50000000000007105, -30.00000000000000000 ) ) ;
#14171 = CARTESIAN_POINT ( 'NONE',  ( 10.73846460100926592, 12.62787417135106161, -222.6344468496098159 ) ) ;
#14172 = CARTESIAN_POINT ( 'NONE',  ( -0.6326494355537284342, -15.87741594504987219, -229.6822519216137266 ) ) ;
#14173 = ORIENTED_EDGE ( 'NONE', *, *, #4962, .F. ) ;
#14174 = CARTESIAN_POINT ( 'NONE',  ( -0.7041916573665241152, 14.60214745152014437, -226.3818583194645555 ) ) ;
#14175 = CARTESIAN_POINT ( 'NONE',  ( -18.09605518090995702, 22.22778748761825085, -222.5443354630425290 ) ) ;
#14176 = CARTESIAN_POINT ( 'NONE',  ( -22.57344584932824105, 14.14390280519600473, -217.2212543695777924 ) ) ;
#14177 = CARTESIAN_POINT ( 'NONE',  ( -13.89163392164661204, -16.46234366268243221, -230.8566716434345949 ) ) ;
#14178 = DIRECTION ( 'NONE',  ( -1.000000000000000000, 0.000000000000000000, 0.000000000000000000 ) ) ;
#14179 = TOROIDAL_SURFACE ( 'NONE', #6607, 24.63401512838747820, 3.000000000000000888 ) ;
#14180 = ORIENTED_EDGE ( 'NONE', *, *, #9431, .T. ) ;
#14181 = CARTESIAN_POINT ( 'NONE',  ( 21.92281339924938877, 16.67475415235398017, -231.9828670874568957 ) ) ;
#14182 = CARTESIAN_POINT ( 'NONE',  ( 7.033108278341462238, -17.71891568601925826, -230.1509483552532060 ) ) ;
#14183 = CARTESIAN_POINT ( 'NONE',  ( 21.39553407250273054, 8.453402029343234148, -217.9531594780983141 ) ) ;
#14184 = CARTESIAN_POINT ( 'NONE',  ( -10.65455960636934662, 10.37188583052882862, -219.5197110153079620 ) ) ;
#14185 = CARTESIAN_POINT ( 'NONE',  ( 29.08100487150598212, 12.14819438347179670, -226.9621620069135020 ) ) ;
#14186 = EDGE_CURVE ( 'NONE', #15384, #1564, #10244, .T. ) ;
#14187 = CARTESIAN_POINT ( 'NONE',  ( 11.82943521288609823, 27.58963564415041247, -226.1180395413371400 ) ) ;
#14188 = FACE_OUTER_BOUND ( 'NONE', #11330, .T. ) ;
#14189 = CARTESIAN_POINT ( 'NONE',  ( -14.84823930505322132, -23.35465403802561823, -218.3226235040776260 ) ) ;
#14190 = CARTESIAN_POINT ( 'NONE',  ( 17.02763684969102798, -14.67205317233652195, -233.2001291093645818 ) ) ;
#14191 = DIRECTION ( 'NONE',  ( 1.000000000000000000, 0.000000000000000000, 0.000000000000000000 ) ) ;
#14192 = TOROIDAL_SURFACE ( 'NONE', #7361, 24.63401512838747820, 3.000000000000000888 ) ;
#14193 = DIRECTION ( 'NONE',  ( 1.000000000000000000, 0.000000000000000000, 0.000000000000000000 ) ) ;
#14194 = CARTESIAN_POINT ( 'NONE',  ( -13.58389614404818069, 15.11490620317918676, -215.3922994348461941 ) ) ;
#14195 = CARTESIAN_POINT ( 'NONE',  ( -21.01940116658287749, -3.333607517048045032, -230.8803659671980597 ) ) ;
#14196 = CARTESIAN_POINT ( 'NONE',  ( -20.97727766418175932, 9.381545086430262970, -232.5968905491617420 ) ) ;
#14197 = CARTESIAN_POINT ( 'NONE',  ( 8.903385417657583289, 10.41040586594612272, -227.6527940987422198 ) ) ;
#14198 = CARTESIAN_POINT ( 'NONE',  ( 5.195682580001069084, 14.86321519495278665, -224.7851167466743334 ) ) ;
#14199 = EDGE_LOOP ( 'NONE', ( #15419, #3190, #7724, #10455 ) ) ;
#14200 = CARTESIAN_POINT ( 'NONE',  ( 20.62543286083822380, -24.26207512693059343, -224.4080524747341201 ) ) ;
#14201 = ORIENTED_EDGE ( 'NONE', *, *, #12149, .F. ) ;
#14202 = CARTESIAN_POINT ( 'NONE',  ( 14.95414693437772868, 8.262206471704862665, -230.1862972580043163 ) ) ;
#14203 = CARTESIAN_POINT ( 'NONE',  ( -23.89856910807799295, 17.42297078648622843, -222.0178620725767757 ) ) ;
#14204 = CARTESIAN_POINT ( 'NONE',  ( -9.251743101293765648, 14.06372330290396278, -232.4239003576353468 ) ) ;
#14205 = CARTESIAN_POINT ( 'NONE',  ( -23.85568197540453994, -15.41036827548725618, -219.8503866864575969 ) ) ;
#14206 = CARTESIAN_POINT ( 'NONE',  ( -22.17339560624464312, 16.26550580028390769, -232.0582861498566274 ) ) ;
#14207 = DIRECTION ( 'NONE',  ( -0.000000000000000000, -0.000000000000000000, 1.000000000000000000 ) ) ;
#14208 = CARTESIAN_POINT ( 'NONE',  ( 17.22423229049764970, 1.395540479540137380, -217.3898520248025363 ) ) ;
#14209 = AXIS2_PLACEMENT_3D ( 'NONE', #1245, #5883, #4194 ) ;
#14210 = CARTESIAN_POINT ( 'NONE',  ( -10.24168223636446662, 16.14271751156598356, -231.4847994864913971 ) ) ;
#14211 = CARTESIAN_POINT ( 'NONE',  ( 9.168912942254459963, 16.03578711007639157, -234.6923200900793347 ) ) ;
#14212 = CARTESIAN_POINT ( 'NONE',  ( -15.23434562258889891, -0.4010941804143903222, -220.4743703065900036 ) ) ;
#14213 = CARTESIAN_POINT ( 'NONE',  ( -12.22852564478610482, -7.025360622849957437, -222.3415469712626589 ) ) ;
#14214 = CARTESIAN_POINT ( 'NONE',  ( 2.601379523478754674, 17.36677895276155681, -230.4357129074444117 ) ) ;
#14215 = CARTESIAN_POINT ( 'NONE',  ( -1.890995374385051608, -13.09686096954197509, -227.5694739903412085 ) ) ;
#14216 = CARTESIAN_POINT ( 'NONE',  ( 7.762960416026701616, 12.60702317161859121, -221.9096828323375235 ) ) ;
#14217 = CARTESIAN_POINT ( 'NONE',  ( 22.52555938611480002, -22.70209057424856525, -227.7033606670069332 ) ) ;
#14218 = CARTESIAN_POINT ( 'NONE',  ( 1.387778780781445676E-13, -19.79999999999999716, -78.50000000000000000 ) ) ;
#14219 = EDGE_CURVE ( 'NONE', #1604, #22159, #1845, .T. ) ;
#14220 = CARTESIAN_POINT ( 'NONE',  ( 17.41909632439413969, 2.006477695503792624, -233.4081875040758121 ) ) ;
#14221 = FILL_AREA_STYLE_COLOUR ( '', #7057 ) ;
#14222 = CARTESIAN_POINT ( 'NONE',  ( 26.86480837698434243, -8.606671353193281249, -231.2046318962545683 ) ) ;
#14223 = CARTESIAN_POINT ( 'NONE',  ( 7.017641603801325623, 14.96204511409594673, -228.1064041248110073 ) ) ;
#14224 = CARTESIAN_POINT ( 'NONE',  ( 21.27683256847563698, 4.223177115764435108, -215.2584548172064842 ) ) ;
#14225 = CARTESIAN_POINT ( 'NONE',  ( 19.20300624114736721, 0.6066039755357417462, -231.5046416827383950 ) ) ;
#14226 = CARTESIAN_POINT ( 'NONE',  ( -14.02540557227298024, -18.71004003062420651, -218.0769645724313932 ) ) ;
#14227 = AXIS2_PLACEMENT_3D ( 'NONE', #3588, #10908, #15869 ) ;
#14228 = CIRCLE ( 'NONE', #2346, 21.63401512838748175 ) ;
#14229 = CARTESIAN_POINT ( 'NONE',  ( 2.892356176081334773, 24.03953794589038395, -215.3901262983647200 ) ) ;
#14230 = CARTESIAN_POINT ( 'NONE',  ( 0.000000000000000000, 0.000000000000000000, -70.00000000000000000 ) ) ;
#14231 = CARTESIAN_POINT ( 'NONE',  ( -6.183400735100206269, -24.17720054222102277, -215.4627583112813625 ) ) ;
#14232 = CARTESIAN_POINT ( 'NONE',  ( -10.91003322996498071, 12.84665145358222382, -229.9786893781767958 ) ) ;
#14233 = EDGE_CURVE ( 'NONE', #16873, #16801, #9157, .T. ) ;
#14234 = CARTESIAN_POINT ( 'NONE',  ( 5.803912621764987456, 13.01725692290267844, -221.8367675400179166 ) ) ;
#14235 = CARTESIAN_POINT ( 'NONE',  ( -20.92673740658815973, 5.672885432599523270, -219.1433548642331459 ) ) ;
#14236 = CARTESIAN_POINT ( 'NONE',  ( 0.9169988354999972779, 20.59043933275470550, -235.2854195559275752 ) ) ;
#14237 = CARTESIAN_POINT ( 'NONE',  ( 19.29259174080182504, 0.5828707127177102931, -219.2781652733668807 ) ) ;
#14238 = CARTESIAN_POINT ( 'NONE',  ( 9.638496285600583136, -13.08983061985817464, -223.8709389748426588 ) ) ;
#14239 = COLOUR_RGB ( '', 0.66274510, 0.83137255, 0.94901961) ;
#14240 = ORIENTED_EDGE ( 'NONE', *, *, #6382, .T. ) ;
#14241 = CARTESIAN_POINT ( 'NONE',  ( 10.05661706967825353, -14.25456047934742365, -218.9909083857680230 ) ) ;
#14242 = CARTESIAN_POINT ( 'NONE',  ( -1.364406401035816785, 24.33111505239456918, -219.5658712396381418 ) ) ;
#14243 = ORIENTED_EDGE ( 'NONE', *, *, #18092, .F. ) ;
#14244 = DIRECTION ( 'NONE',  ( -0.000000000000000000, -1.000000000000000000, -0.000000000000000000 ) ) ;
#14245 = CARTESIAN_POINT ( 'NONE',  ( 25.80927844399814930, 11.21489550116160316, -221.3538377621514996 ) ) ;
#14246 = CARTESIAN_POINT ( 'NONE',  ( -26.73251495235368225, -0.6309583860051256599, -232.5016102969711085 ) ) ;
#14247 = CARTESIAN_POINT ( 'NONE',  ( -18.89430729770302975, -12.42271633246521212, -233.2230176520695295 ) ) ;
#14248 = CARTESIAN_POINT ( 'NONE',  ( -8.379125946468517938, -29.31735857037017468, -221.8060643354269814 ) ) ;
#14249 = CARTESIAN_POINT ( 'NONE',  ( -9.106229537879125147, 25.89784491087598184, -228.9807674929363372 ) ) ;
#14250 = CARTESIAN_POINT ( 'NONE',  ( 0.000000000000000000, -23.00000000000006040, -60.00000000000000000 ) ) ;
#14251 = CARTESIAN_POINT ( 'NONE',  ( 15.54095364727189299, 10.52000078266145700, -230.2714373371992735 ) ) ;
#14252 = CARTESIAN_POINT ( 'NONE',  ( -8.172572110426221670, 16.86653848210977813, -233.4220330256369493 ) ) ;
#14253 = CARTESIAN_POINT ( 'NONE',  ( -13.40354389326479456, 23.35336998323175450, -219.8517474526506987 ) ) ;
#14254 = MANIFOLD_SOLID_BREP ( 'Sweep2', #2168 ) ;
#14255 = ORIENTED_EDGE ( 'NONE', *, *, #17479, .F. ) ;
#14256 = CARTESIAN_POINT ( 'NONE',  ( 1.104227501629593045, 25.05528885094460989, -231.9808705443460326 ) ) ;
#14257 = CARTESIAN_POINT ( 'NONE',  ( -25.17056316833229701, 11.10725809642625705, -227.0225660235207386 ) ) ;
#14258 = CARTESIAN_POINT ( 'NONE',  ( 12.71499452845021416, 2.172589307656224378, -223.9381607050773084 ) ) ;
#14259 = CARTESIAN_POINT ( 'NONE',  ( 6.755953262402430326, -28.44658494672641424, -224.7309905328439754 ) ) ;
#14261 = CARTESIAN_POINT ( 'NONE',  ( 21.04928763009552384, -0.2309942901367783852, -233.9427286327411366 ) ) ;
#14260 = CIRCLE ( 'NONE', #9225, 25.00000000000001066 ) ;
#14262 = ORIENTED_EDGE ( 'NONE', *, *, #10571, .T. ) ;
#14263 = CARTESIAN_POINT ( 'NONE',  ( 10.85888002857596923, 15.81835858589122878, -232.3913150909872627 ) ) ;
#14264 = CARTESIAN_POINT ( 'NONE',  ( 27.03411061974195562, -3.460823241630351710, -221.7771387205989413 ) ) ;
#14265 = CARTESIAN_POINT ( 'NONE',  ( 15.09054553479285588, -1.912330756057289527, -222.3157747520536702 ) ) ;
#14266 = EDGE_CURVE ( 'NONE', #15933, #12371, #8616, .T. ) ;
#14267 = CARTESIAN_POINT ( 'NONE',  ( 10.30328786010431052, -20.08430705480546408, -216.1847100135515802 ) ) ;
#14268 = CARTESIAN_POINT ( 'NONE',  ( -19.00318367631585659, 13.14621133775862916, -233.8403879275295765 ) ) ;
#14269 = AXIS2_PLACEMENT_3D ( 'NONE', #3777, #10659, #17525 ) ;
#14270 = CARTESIAN_POINT ( 'NONE',  ( -9.578110717394128670, 23.64032677849093034, -215.7669555765890550 ) ) ;
#14271 = VERTEX_POINT ( 'NONE', #20745 ) ;
#14272 = CARTESIAN_POINT ( 'NONE',  ( -11.69688825528096388, 18.63404371591177622, -215.8612738028812714 ) ) ;
#14273 = CARTESIAN_POINT ( 'NONE',  ( -11.96453848309674228, -6.796862595549911568, -223.8262896469332759 ) ) ;
#14274 = LINE ( 'NONE', #417, #6588 ) ;
#14275 = CARTESIAN_POINT ( 'NONE',  ( -21.95886157946472750, 6.845920284573796089, -7.296501936155945778 ) ) ;
#14276 = CARTESIAN_POINT ( 'NONE',  ( -16.74550766701807447, 3.787526820511904813, -217.9802846976114381 ) ) ;
#14277 = CARTESIAN_POINT ( 'NONE',  ( 0.5037192024386412115, -21.28831724695581684, -215.7417742237681466 ) ) ;
#14278 = CARTESIAN_POINT ( 'NONE',  ( 23.74723497152361062, 5.524508269105988134, -217.6012181427065002 ) ) ;
#14279 = CARTESIAN_POINT ( 'NONE',  ( -23.70973587455150522, 20.45398817402440983, -228.9005348699235469 ) ) ;
#14280 = DIRECTION ( 'NONE',  ( -0.000000000000000000, -0.000000000000000000, 1.000000000000000000 ) ) ;
#14281 = CARTESIAN_POINT ( 'NONE',  ( 12.51085646230496273, 9.582567546749562126, -224.6200301875240939 ) ) ;
#14282 = CARTESIAN_POINT ( 'NONE',  ( 5.681636183907174065, -27.87860296351749767, -230.4665658140699804 ) ) ;
#14283 = ORIENTED_EDGE ( 'NONE', *, *, #13899, .F. ) ;
#14284 = CARTESIAN_POINT ( 'NONE',  ( 3.219568897812384645, 28.82511222849302257, -221.5626884747494216 ) ) ;
#14285 = CARTESIAN_POINT ( 'NONE',  ( -11.69222874857179484, 25.57550432052970280, -219.9467848335519591 ) ) ;
#14286 = CARTESIAN_POINT ( 'NONE',  ( -15.00242079508237936, 7.335218745534954898, -232.9526071471669013 ) ) ;
#14287 = ORIENTED_EDGE ( 'NONE', *, *, #13072, .F. ) ;
#14288 = CARTESIAN_POINT ( 'NONE',  ( -12.03049011398204726, -11.12540611457240480, -223.2385418847515268 ) ) ;
#14289 = CARTESIAN_POINT ( 'NONE',  ( 0.000000000000000000, 0.000000000000000000, -126.0000000000000284 ) ) ;
#14290 = VERTEX_POINT ( 'NONE', #12208 ) ;
#14291 = CARTESIAN_POINT ( 'NONE',  ( -17.84981083811007707, 0.8485253248287054628, -231.8041300026935119 ) ) ;
#14292 = CARTESIAN_POINT ( 'NONE',  ( 0.5598654370342924791, -17.79304497667748564, -219.0037976856824571 ) ) ;
#14293 = CARTESIAN_POINT ( 'NONE',  ( 17.60676319847677007, 21.31475060840986302, -219.8266339603936785 ) ) ;
#14294 = CARTESIAN_POINT ( 'NONE',  ( 4.389496648589924277, 14.47660514356954131, -220.6151178996808540 ) ) ;
#14295 = MANIFOLD_SOLID_BREP ( 'Revolve1', #17930 ) ;
#14296 = CARTESIAN_POINT ( 'NONE',  ( 15.87399429023076003, -1.683916961781461552, -230.8621029165058758 ) ) ;
#14297 = CARTESIAN_POINT ( 'NONE',  ( 4.343013938751969505, 13.02036404005131587, -224.7825435359082178 ) ) ;
#14298 = CYLINDRICAL_SURFACE ( 'NONE', #10912, 20.99999999999999645 ) ;
#14299 = CARTESIAN_POINT ( 'NONE',  ( -10.42804209284631156, -14.08702332024887305, -217.7386024361820489 ) ) ;
#14300 = CARTESIAN_POINT ( 'NONE',  ( 14.18709644517307922, -11.45356969546147496, -232.2178450427173004 ) ) ;
#14301 = DIRECTION ( 'NONE',  ( -0.000000000000000000, -0.000000000000000000, 1.000000000000000000 ) ) ;
#14302 = CARTESIAN_POINT ( 'NONE',  ( 1.232595164407830946E-29, -17.50000000000007105, -24.99999999999999645 ) ) ;
#14303 = CARTESIAN_POINT ( 'NONE',  ( -16.38161496430853248, 17.22219235543852989, -215.3343469598664797 ) ) ;
#14304 = CARTESIAN_POINT ( 'NONE',  ( -21.95460872137175201, -8.074699112730320039, -230.7190249947325071 ) ) ;
#14305 = CARTESIAN_POINT ( 'NONE',  ( -13.37045227479810094, 5.250293981428504786, -224.2914120185227205 ) ) ;
#14306 = CARTESIAN_POINT ( 'NONE',  ( 15.88043104796248528, 11.88135572392608807, -216.2525917828042168 ) ) ;
#14307 = CARTESIAN_POINT ( 'NONE',  ( -2.117958212721558375, 27.20243410318316535, -230.7086725634165418 ) ) ;
#14308 = ORIENTED_EDGE ( 'NONE', *, *, #17232, .F. ) ;
#14309 = CARTESIAN_POINT ( 'NONE',  ( 10.59985392024617745, -10.68425835910226418, -232.2123170752960277 ) ) ;
#14310 = CARTESIAN_POINT ( 'NONE',  ( 26.48990917286906921, 12.16675355942207659, -225.0153622588060216 ) ) ;
#14311 = CARTESIAN_POINT ( 'NONE',  ( -2.577721557973523314, 25.83760098923793791, -215.4660676095525389 ) ) ;
#14312 = EDGE_CURVE ( 'NONE', #16331, #15940, #6640, .T. ) ;
#14313 = CARTESIAN_POINT ( 'NONE',  ( -13.25293905438448405, 17.39325876214774524, -215.6628841494472510 ) ) ;
#14314 = CARTESIAN_POINT ( 'NONE',  ( -13.36955836198420577, -3.222265253903016990, -227.4060678739157026 ) ) ;
#14315 = CARTESIAN_POINT ( 'NONE',  ( -9.250876228778270871, 9.538614635316015722, -227.1332118982684563 ) ) ;
#14316 = CARTESIAN_POINT ( 'NONE',  ( -11.40691176929435535, -8.999942255032468807, 93.00000000000000000 ) ) ;
#14317 = CARTESIAN_POINT ( 'NONE',  ( 17.95694455891925756, -3.510678534943489026, -231.2643001502910067 ) ) ;
#14318 = CARTESIAN_POINT ( 'NONE',  ( -12.70465517376339193, 12.03139199664008530, -229.6235454691090752 ) ) ;
#14319 = CARTESIAN_POINT ( 'NONE',  ( -18.93763370444446181, -0.7340653299870684156, -219.7345063954518594 ) ) ;
#14320 = CARTESIAN_POINT ( 'NONE',  ( 28.62253243811995418, 3.652502539191337494, -225.4068779441649326 ) ) ;
#14321 = CARTESIAN_POINT ( 'NONE',  ( 15.91295838535984331, 21.88410254487826379, -230.9583961155862823 ) ) ;
#14322 = CARTESIAN_POINT ( 'NONE',  ( -12.65123680455331190, -6.798726433138870817, -228.2089845657881710 ) ) ;
#14323 = VERTEX_POINT ( 'NONE', #10410 ) ;
#14324 = CARTESIAN_POINT ( 'NONE',  ( 0.7903203334012884884, 21.30772501796948859, -217.9064416298261619 ) ) ;
#14325 = CARTESIAN_POINT ( 'NONE',  ( -3.300598509645395584, -18.18730530649546395, -233.4303386612170925 ) ) ;
#14326 = CARTESIAN_POINT ( 'NONE',  ( 18.23324537670537993, 23.47692953258263771, -224.8333321331434433 ) ) ;
#14327 = CARTESIAN_POINT ( 'NONE',  ( 5.002389762228888870, -13.81148461055073362, -218.0662212534467983 ) ) ;
#14328 = DIRECTION ( 'NONE',  ( 0.03647168421188083653, 0.3315607655626302552, 0.9427286327412950362 ) ) ;
#14329 = CARTESIAN_POINT ( 'NONE',  ( -10.16319438574952372, 11.71174522937666040, -227.8434026503654479 ) ) ;
#14330 = CARTESIAN_POINT ( 'NONE',  ( 24.64273247744971229, -10.07127014888436278, -217.7281412196979602 ) ) ;
#14331 = CARTESIAN_POINT ( 'NONE',  ( 3.060417506408009469, 27.46204888741655026, -226.6022202862033623 ) ) ;
#14332 = CARTESIAN_POINT ( 'NONE',  ( -18.94992041651601156, 14.87246523864368974, -232.0280096192260828 ) ) ;
#14334 = VECTOR ( 'NONE', #8854, 1000.000000000000000 ) ;
#14333 = CARTESIAN_POINT ( 'NONE',  ( -20.87212828950092813, -0.8819659211619411687, -215.0000000018925448 ) ) ;
#14335 = CARTESIAN_POINT ( 'NONE',  ( -13.33153391309230074, -13.53657406488594184, -231.3594229707590557 ) ) ;
#14336 = CARTESIAN_POINT ( 'NONE',  ( 15.65443801613259467, 7.488839228060037989, -233.6469817377710569 ) ) ;
#14337 = FACE_OUTER_BOUND ( 'NONE', #15543, .T. ) ;
#14338 = CARTESIAN_POINT ( 'NONE',  ( 0.3570725323625942860, -15.31465789365257102, -218.3993834748477525 ) ) ;
#14339 = CARTESIAN_POINT ( 'NONE',  ( 10.25948093768852054, 28.38842464930171872, -224.3436940787075855 ) ) ;
#14340 = CARTESIAN_POINT ( 'NONE',  ( 10.95881707662767290, 12.06788758096456782, -231.4359029166177208 ) ) ;
#14341 = EDGE_CURVE ( 'NONE', #2064, #8296, #884, .T. ) ;
#14342 = CARTESIAN_POINT ( 'NONE',  ( -13.14888680331901583, 26.03314517226533908, -227.7900104434697539 ) ) ;
#14343 = AXIS2_PLACEMENT_3D ( 'NONE', #18998, #12587, #4017 ) ;
#14344 = CARTESIAN_POINT ( 'NONE',  ( -5.467362224022371819, 23.92882567691090046, -234.7811165710531611 ) ) ;
#14345 = CARTESIAN_POINT ( 'NONE',  ( 27.50364976068844669, 3.973406265104437729, -228.8805639113908228 ) ) ;
#14346 = ORIENTED_EDGE ( 'NONE', *, *, #8177, .F. ) ;
#14347 = CARTESIAN_POINT ( 'NONE',  ( 11.43327405580198608, -14.46863304034511799, -220.4355838810013495 ) ) ;
#14348 = ORIENTED_EDGE ( 'NONE', *, *, #12996, .T. ) ;
#14349 = CARTESIAN_POINT ( 'NONE',  ( 9.037704487505543227, -20.74919929927824214, -217.6023494967207625 ) ) ;
#14350 = CARTESIAN_POINT ( 'NONE',  ( -3.926352947695993745, 17.69140300707508473, -220.1607884481205986 ) ) ;
#14351 = DIRECTION ( 'NONE',  ( -1.000000000000000000, 0.000000000000000000, 0.000000000000000000 ) ) ;
#14352 = CARTESIAN_POINT ( 'NONE',  ( 15.52719855059926424, 1.633696074270991172, -221.7349885876216433 ) ) ;
#14353 = CARTESIAN_POINT ( 'NONE',  ( 23.48720700658024896, -2.145453947144424500, -217.8824464111000054 ) ) ;
#14354 = CARTESIAN_POINT ( 'NONE',  ( -11.36971918743327237, -8.287084598727400220, -223.1364763414170227 ) ) ;
#14355 = CARTESIAN_POINT ( 'NONE',  ( 8.115778909262310492, -29.92983049028717346, -224.5060555478150377 ) ) ;
#14356 = CARTESIAN_POINT ( 'NONE',  ( 3.614175329767659761, 21.98488100320606264, -219.0898850257099753 ) ) ;
#14357 = DIRECTION ( 'NONE',  ( 0.1736481776669307198, 0.000000000000000000, 0.9848077530122080203 ) ) ;
#14358 = CARTESIAN_POINT ( 'NONE',  ( -15.64716994811699813, 6.210654946517923491, -217.0002936794128345 ) ) ;
#14359 = CARTESIAN_POINT ( 'NONE',  ( -12.90983082593748676, 14.84936372681532823, -233.8009687022269532 ) ) ;
#14360 = CARTESIAN_POINT ( 'NONE',  ( -2.554014161526931392, 17.56271496069470572, -229.4905841158208659 ) ) ;
#14361 = ORIENTED_EDGE ( 'NONE', *, *, #2596, .F. ) ;
#14362 = CARTESIAN_POINT ( 'NONE',  ( 23.44028133050380802, 19.87677100428751231, -223.1503774981096342 ) ) ;
#14363 = CARTESIAN_POINT ( 'NONE',  ( -15.15469129103955304, 15.56563882170958024, -231.6314069158229643 ) ) ;
#14364 = CARTESIAN_POINT ( 'NONE',  ( 30.65249971456167799, 3.724008896938769464, -225.4815109119605552 ) ) ;
#14365 = CARTESIAN_POINT ( 'NONE',  ( -1.097449620509919788, -25.21235133823365260, -218.6697740411501059 ) ) ;
#14366 = FACE_OUTER_BOUND ( 'NONE', #22036, .T. ) ;
#14367 = ORIENTED_EDGE ( 'NONE', *, *, #5873, .T. ) ;
#14368 = CARTESIAN_POINT ( 'NONE',  ( 4.340445191644851874, 29.86837761166362881, -227.4879512554873315 ) ) ;
#14369 = CARTESIAN_POINT ( 'NONE',  ( -31.58308234758948174, -0.5371106682196264970, -221.7519263543700845 ) ) ;
#14370 = DIRECTION ( 'NONE',  ( -1.000000000000000000, 0.000000000000000000, 0.000000000000000000 ) ) ;
#14371 = CARTESIAN_POINT ( 'NONE',  ( -0.1947256686167265494, -30.94043057420685727, -223.1178397439027492 ) ) ;
#14372 = PRODUCT_CONTEXT ( 'NONE', #6851, 'mechanical' ) ;
#14373 = CARTESIAN_POINT ( 'NONE',  ( -10.51143808951550085, 11.41308718311005066, -231.3573069600382439 ) ) ;
#14374 = CARTESIAN_POINT ( 'NONE',  ( -7.403072389817287657, 18.92851032520892929, -215.2068968469505137 ) ) ;
#14375 = EDGE_LOOP ( 'NONE', ( #8482, #8691, #14397, #9393 ) ) ;
#14376 = CARTESIAN_POINT ( 'NONE',  ( -9.151299407007059017, 9.196974979111923076, -223.9483834032048719 ) ) ;
#14377 = CARTESIAN_POINT ( 'NONE',  ( -24.78729321827560739, -16.46449136890227294, -222.3867555963062443 ) ) ;
#14378 = LINE ( 'NONE', #21106, #2626 ) ;
#14379 = CARTESIAN_POINT ( 'NONE',  ( -22.94233912960511645, 1.659357271331404871, -9.866832502321154053 ) ) ;
#14380 = CARTESIAN_POINT ( 'NONE',  ( -18.47334320050258327, 24.79293862780133040, -226.9986786077537317 ) ) ;
#14381 = CARTESIAN_POINT ( 'NONE',  ( 3.568716337251232051, -21.91366830329386772, -233.6537821856145172 ) ) ;
#14382 = CARTESIAN_POINT ( 'NONE',  ( 17.50000000000000355, 0.000000000000000000, -70.00000000000000000 ) ) ;
#14383 = CARTESIAN_POINT ( 'NONE',  ( -22.99617382825321599, 17.18101613848176967, -230.9512687019100099 ) ) ;
#14384 = CARTESIAN_POINT ( 'NONE',  ( 20.22510869507564024, 17.05975164568011238, -220.7829296213589316 ) ) ;
#14385 = EDGE_CURVE ( 'NONE', #17378, #20879, #6267, .T. ) ;
#14386 = CARTESIAN_POINT ( 'NONE',  ( 5.365126951644291431, 19.60085171667039816, -218.9155869426879519 ) ) ;
#14387 = DIRECTION ( 'NONE',  ( 1.000000000000000000, 6.982962677686266711E-15, 0.000000000000000000 ) ) ;
#14388 = CARTESIAN_POINT ( 'NONE',  ( 14.40184562439531213, 6.414772937171507650, -227.4651811604036595 ) ) ;
#14389 = CARTESIAN_POINT ( 'NONE',  ( -14.65844530258765310, -17.20867344037294444, -230.8340913472024170 ) ) ;
#14390 = EDGE_LOOP ( 'NONE', ( #14201, #10958, #1336, #19783 ) ) ;
#14391 = EDGE_CURVE ( 'NONE', #15638, #16686, #19496, .T. ) ;
#14392 = CARTESIAN_POINT ( 'NONE',  ( -0.5888410438786807477, 14.99789765555501475, -227.7044550383138244 ) ) ;
#14393 = CARTESIAN_POINT ( 'NONE',  ( -11.55316006017064012, 19.79513644261079719, -232.3088878043970453 ) ) ;
#14394 = CARTESIAN_POINT ( 'NONE',  ( -8.112279890008961658, 11.99566605360304727, -225.9834628568286519 ) ) ;
#14395 = CARTESIAN_POINT ( 'NONE',  ( -20.35224420216377439, -13.00389602580315085, -219.1266045330881980 ) ) ;
#14396 = CARTESIAN_POINT ( 'NONE',  ( 0.000000000000000000, 0.000000000000000000, -20.00000000000000000 ) ) ;
#14397 = ORIENTED_EDGE ( 'NONE', *, *, #19790, .F. ) ;
#14398 = CARTESIAN_POINT ( 'NONE',  ( -15.23434562258889891, -0.4010941804143903222, -220.4743703065900036 ) ) ;
#14399 = CARTESIAN_POINT ( 'NONE',  ( -0.6467335922136470128, -17.26771294536504442, -230.4732896975262122 ) ) ;
#14400 = CARTESIAN_POINT ( 'NONE',  ( 12.85408565574548412, 7.821283853063205171, -223.1248833997948111 ) ) ;
#14401 = CARTESIAN_POINT ( 'NONE',  ( 0.7245137624042983227, 13.44764381486384330, -223.4043886706536455 ) ) ;
#14402 = PRODUCT_DEFINITION_CONTEXT ( 'detailed design', #8297, 'design' ) ;
#14403 = CARTESIAN_POINT ( 'NONE',  ( -15.12838653695630420, 3.161599240781852949, -225.7834014684609656 ) ) ;
#14404 = CARTESIAN_POINT ( 'NONE',  ( 12.56362091610784049, 9.747446748398973071, -231.6428467497164547 ) ) ;
#14405 = CARTESIAN_POINT ( 'NONE',  ( 13.43730899468209294, 8.427513769504761498, -221.4030804848920297 ) ) ;
#14406 = CARTESIAN_POINT ( 'NONE',  ( -4.100000000000000533, 5.021051876504148371E-16, -103.0000000000000000 ) ) ;
#14407 = CARTESIAN_POINT ( 'NONE',  ( -15.74157322273402748, -13.22745315869835636, -216.7831660370879661 ) ) ;
#14408 = CARTESIAN_POINT ( 'NONE',  ( 2.178520447619924472, -13.56847537563065487, -221.4085897031499428 ) ) ;
#14409 = LINE ( 'NONE', #2783, #13137 ) ;
#14410 = DIRECTION ( 'NONE',  ( -0.000000000000000000, 0.000000000000000000, -1.000000000000000000 ) ) ;
#14411 = CARTESIAN_POINT ( 'NONE',  ( -11.10543627608095285, 3.497967533612860613, -224.1342318769322617 ) ) ;
#14412 = CARTESIAN_POINT ( 'NONE',  ( 18.88835481822873774, -3.841660717124094848, -234.8883833189080974 ) ) ;
#14413 = CARTESIAN_POINT ( 'NONE',  ( 14.69853173970351179, 23.44775873627089524, -231.2711109634281001 ) ) ;
#14414 = CARTESIAN_POINT ( 'NONE',  ( 8.162622027327667951, 13.88735946031204094, -224.7165241036068153 ) ) ;
#14415 = VERTEX_POINT ( 'NONE', #19609 ) ;
#14416 = CARTESIAN_POINT ( 'NONE',  ( 11.82206472115893447, -5.594380913675770728, -219.9420363600394239 ) ) ;
#14417 = CARTESIAN_POINT ( 'NONE',  ( 17.99029889091409018, 9.613712288440757092, -232.0298403238024036 ) ) ;
#14418 = CARTESIAN_POINT ( 'NONE',  ( -0.4465333940385243228, 12.27026616490476485, -221.3722328744566425 ) ) ;
#14419 = CARTESIAN_POINT ( 'NONE',  ( -18.70090456008720992, 23.36146401084868884, -220.3989740370807056 ) ) ;
#14420 = CARTESIAN_POINT ( 'NONE',  ( -17.04082806826102470, -4.797954729550726327, -217.3726213297937306 ) ) ;
#14421 = CARTESIAN_POINT ( 'NONE',  ( -11.98736441306973077, 11.45674391201457176, -217.8252237716743025 ) ) ;
#14422 = CARTESIAN_POINT ( 'NONE',  ( 9.901812489146273322, -10.59772277891044290, 93.00000000000000000 ) ) ;
#14423 = CARTESIAN_POINT ( 'NONE',  ( 26.48152825632016061, -2.044474411990439666, -219.3412966555575565 ) ) ;
#14424 = PRODUCT_RELATED_PRODUCT_CATEGORY ( 'part', '', ( #17154 ) ) ;
#14425 = CARTESIAN_POINT ( 'NONE',  ( 1.898427734299754421, 12.47096978853034521, -227.5043976727869506 ) ) ;
#14426 = CARTESIAN_POINT ( 'NONE',  ( 20.96405783751201213, 6.249056650590980588, -215.6254004080763309 ) ) ;
#14427 = CARTESIAN_POINT ( 'NONE',  ( -23.52999999174766543, 19.39566142560855866, -221.9446938626390704 ) ) ;
#14428 = CARTESIAN_POINT ( 'NONE',  ( 4.301648988406530094, 13.23079486486395240, -223.2766268961034655 ) ) ;
#14429 = DIRECTION ( 'NONE',  ( 1.000000000000000000, 0.000000000000000000, 0.000000000000000000 ) ) ;
#14430 = CARTESIAN_POINT ( 'NONE',  ( 5.466128392039544259, 27.94759090250835243, -223.5617905851570981 ) ) ;
#14431 = CARTESIAN_POINT ( 'NONE',  ( -9.606889355748592152, -11.26588727105406385, -229.9123324032181586 ) ) ;
#14432 = CARTESIAN_POINT ( 'NONE',  ( 11.13678936984666912, 26.95732789089726111, -228.8350761760834757 ) ) ;
#14433 = CARTESIAN_POINT ( 'NONE',  ( 22.36312131198404174, -23.32398317548372546, -224.0789201928890861 ) ) ;
#14434 = CARTESIAN_POINT ( 'NONE',  ( 20.62542899963660759, 1.332263963074341584, -222.3060979289667216 ) ) ;
#14435 = CARTESIAN_POINT ( 'NONE',  ( -24.39036648059286350, 13.21953970265592027, -220.1632778389106591 ) ) ;
#14436 = CARTESIAN_POINT ( 'NONE',  ( 16.80562970167152415, -4.609754314392994878, -232.4812892975905356 ) ) ;
#14437 = CARTESIAN_POINT ( 'NONE',  ( 9.425340689562565544, 25.38932416188112384, -221.3391712389563963 ) ) ;
#14438 = CARTESIAN_POINT ( 'NONE',  ( -17.99720854823001659, 13.97888873227035056, -232.2992184661552244 ) ) ;
#14439 = CARTESIAN_POINT ( 'NONE',  ( 19.19288224840068935, 10.13059690604263174, -232.1906135022504998 ) ) ;
#14440 = CARTESIAN_POINT ( 'NONE',  ( -11.58793217866213787, -13.88438693436061477, -219.4860661588769801 ) ) ;
#14441 = CARTESIAN_POINT ( 'NONE',  ( 24.61409543538958289, 19.88121288930873476, -228.5015986536257344 ) ) ;
#14442 = DIRECTION ( 'NONE',  ( 0.000000000000000000, 6.938893903907222461E-16, 1.000000000000000000 ) ) ;
#14443 = CARTESIAN_POINT ( 'NONE',  ( -23.03165807712271373, -11.67016847039487892, -215.7330867557714384 ) ) ;
#14444 = CARTESIAN_POINT ( 'NONE',  ( 2.535512286608554433, 13.86868953312499109, -224.9313928733152181 ) ) ;
#14445 = CARTESIAN_POINT ( 'NONE',  ( 20.10109416526603709, 2.018147939476731434, -216.1034161917718848 ) ) ;
#14446 = VECTOR ( 'NONE', #1503, 1000.000000000000000 ) ;
#14447 = CARTESIAN_POINT ( 'NONE',  ( -12.80756961294691010, 26.82110654133967387, -223.7464923486294026 ) ) ;
#14448 = CARTESIAN_POINT ( 'NONE',  ( -12.80532875684362715, 24.61139456694233374, -232.5885756414849084 ) ) ;
#14449 = CARTESIAN_POINT ( 'NONE',  ( 20.54442553493903389, -1.409480604460696007, -231.2888200459364327 ) ) ;
#14450 = CARTESIAN_POINT ( 'NONE',  ( 0.4541713596374759021, -15.35025901140449989, -222.0332685144132370 ) ) ;
#14451 = ORIENTED_EDGE ( 'NONE', *, *, #8739, .F. ) ;
#14452 = CARTESIAN_POINT ( 'NONE',  ( 5.380811198380419214, -14.52623441703906160, -221.9013399998540024 ) ) ;
#14453 = DIRECTION ( 'NONE',  ( 0.000000000000000000, 0.000000000000000000, 1.000000000000000000 ) ) ;
#14454 = AXIS2_PLACEMENT_3D ( 'NONE', #6453, #11416, #16590 ) ;
#14455 = CARTESIAN_POINT ( 'NONE',  ( 26.24002132888527328, 11.62331517472360964, -222.5300873157218859 ) ) ;
#14456 = CARTESIAN_POINT ( 'NONE',  ( 28.78651053433536333, -0.9604905981993369091, -227.3547688931310233 ) ) ;
#14457 = CARTESIAN_POINT ( 'NONE',  ( -15.74157322273402748, -13.22745315869835636, -216.7831660370879661 ) ) ;
#14458 = CARTESIAN_POINT ( 'NONE',  ( -6.722478243781921492, -14.20656108661463612, -231.4169491518476889 ) ) ;
#14459 = CARTESIAN_POINT ( 'NONE',  ( 3.786538429322381383, 16.06208591393598084, -226.9891439814428793 ) ) ;
#14460 = CARTESIAN_POINT ( 'NONE',  ( 1.322875655532295358, 1.500000000000000000, -120.0000000000000000 ) ) ;
#14461 = CARTESIAN_POINT ( 'NONE',  ( -13.33011381921379090, 5.829915729572584304, -219.4453182727427816 ) ) ;
#14462 = CARTESIAN_POINT ( 'NONE',  ( -6.571166997218196748, 12.74865329367398736, -229.9840124400968762 ) ) ;
#14463 = CARTESIAN_POINT ( 'NONE',  ( 3.786538429322381383, 16.06208591393598084, -226.9891439814428793 ) ) ;
#14464 = CARTESIAN_POINT ( 'NONE',  ( 13.62633932172415641, -0.5436634383532278347, -227.0682007726617542 ) ) ;
#14465 = EDGE_LOOP ( 'NONE', ( #6477, #3465, #6397, #20070 ) ) ;
#14466 = CARTESIAN_POINT ( 'NONE',  ( 16.55626903245587656, 22.80423546114836952, -218.9884947126587633 ) ) ;
#14467 = CARTESIAN_POINT ( 'NONE',  ( -18.36252859017411510, 21.06344830687906367, -228.5073589488702623 ) ) ;
#14468 = CARTESIAN_POINT ( 'NONE',  ( 14.54999166170408209, 3.068772298969228096, -219.4784171371563275 ) ) ;
#14469 = CARTESIAN_POINT ( 'NONE',  ( 2.936803900436826709, -18.74190719154852758, -218.5197582523356061 ) ) ;
#14470 = CARTESIAN_POINT ( 'NONE',  ( 0.000000000000000000, -23.00000000000000000, 75.00000000000000000 ) ) ;
#14471 = CARTESIAN_POINT ( 'NONE',  ( 0.000000000000000000, 0.000000000000000000, 75.00000000000000000 ) ) ;
#14472 = AXIS2_PLACEMENT_3D ( 'NONE', #3695, #558, #10580 ) ;
#14473 = CARTESIAN_POINT ( 'NONE',  ( 6.093530912645064745, 16.79941505724243811, -232.1766444656230419 ) ) ;
#14474 = CARTESIAN_POINT ( 'NONE',  ( 15.57890332219703389, -7.739300371747003027, -228.5080386124398899 ) ) ;
#14475 = DIRECTION ( 'NONE',  ( -6.123233995736766036E-17, 0.000000000000000000, 1.000000000000000000 ) ) ;
#14476 = CARTESIAN_POINT ( 'NONE',  ( -15.17658589853145479, -26.64966442869902252, -226.8090782225333442 ) ) ;
#14477 = APPLICATION_CONTEXT ( 'automotive_design' ) ;
#14478 = CARTESIAN_POINT ( 'NONE',  ( -3.205260335674071648, 17.52234722004434531, -232.9754319808710363 ) ) ;
#14479 = CARTESIAN_POINT ( 'NONE',  ( 4.401501667365108617, 18.53594119471695123, -215.1186850315663150 ) ) ;
#14480 = ORIENTED_EDGE ( 'NONE', *, *, #13596, .F. ) ;
#14481 = CARTESIAN_POINT ( 'NONE',  ( -22.04257564474043818, 18.72061943465525857, -219.1781831295219263 ) ) ;
#14482 = CARTESIAN_POINT ( 'NONE',  ( -10.35216574861945560, -14.43870810227675605, -231.1876371800402126 ) ) ;
#14483 = DIRECTION ( 'NONE',  ( 1.000000000000000000, 0.000000000000000000, 0.000000000000000000 ) ) ;
#14484 = CARTESIAN_POINT ( 'NONE',  ( -20.74377437872641394, 9.935632711291296104, -1.314056478963706365 ) ) ;
#14485 = CARTESIAN_POINT ( 'NONE',  ( -2.735889804569492600, 12.71735652435744512, -225.1194195722198117 ) ) ;
#14486 = CARTESIAN_POINT ( 'NONE',  ( 2.478093603766003294, -30.50979708220057063, -227.6059245187310012 ) ) ;
#14487 = AXIS2_PLACEMENT_3D ( 'NONE', #16394, #8070, #973 ) ;
#14488 = CARTESIAN_POINT ( 'NONE',  ( -23.06814834742187514, 0.000000000000000000, -74.48236190979496030 ) ) ;
#14489 = CARTESIAN_POINT ( 'NONE',  ( -13.55591840520136770, 8.363404288414606924, -231.2690188357804857 ) ) ;
#14490 = CIRCLE ( 'NONE', #4057, 3.000000000000002665 ) ;
#14491 = CARTESIAN_POINT ( 'NONE',  ( -16.40095417437164471, 2.582410108382750646, -233.5151473761628154 ) ) ;
#14492 = CARTESIAN_POINT ( 'NONE',  ( -1.243734262319729389, 14.23902626181890518, -226.4313640849764795 ) ) ;
#14493 = DIRECTION ( 'NONE',  ( -0.000000000000000000, -0.000000000000000000, 1.000000000000000000 ) ) ;
#14494 = CARTESIAN_POINT ( 'NONE',  ( 17.02590609996173754, 6.796709046606974169, -230.8496778635019098 ) ) ;
#14495 = CARTESIAN_POINT ( 'NONE',  ( -8.081326109241135924, -15.70152450856234871, -229.3783721713404304 ) ) ;
#14496 = EDGE_CURVE ( 'NONE', #1365, #15746, #19559, .T. ) ;
#14497 = ORIENTED_EDGE ( 'NONE', *, *, #10591, .T. ) ;
#14498 = CARTESIAN_POINT ( 'NONE',  ( 14.69853173970351179, 23.44775873627089524, -231.2711109634281001 ) ) ;
#14499 = CARTESIAN_POINT ( 'NONE',  ( -6.804439720554941395, 15.25609613835249156, -218.7834354895107651 ) ) ;
#14500 = CARTESIAN_POINT ( 'NONE',  ( -11.88513743913613752, 17.65694776598872195, -232.6054623148957035 ) ) ;
#14501 = CARTESIAN_POINT ( 'NONE',  ( -24.12156516248416693, -2.505154625461648799, -217.3585533157102248 ) ) ;
#14502 = CARTESIAN_POINT ( 'NONE',  ( 13.12488928717151637, 1.903064858314465868E-15, -105.0000000000000000 ) ) ;
#14503 = ORIENTED_EDGE ( 'NONE', *, *, #13039, .T. ) ;
#14504 = CARTESIAN_POINT ( 'NONE',  ( -20.26851768784797869, -0.8260594303982465858, -217.1279713726092098 ) ) ;
#14505 = CARTESIAN_POINT ( 'NONE',  ( 6.592356972974974916, -14.93599889844929862, -226.9608163220883625 ) ) ;
#14506 = FACE_OUTER_BOUND ( 'NONE', #7584, .T. ) ;
#14507 = CARTESIAN_POINT ( 'NONE',  ( -2.808235066048971440, 30.42019778760651150, -222.6481917607299295 ) ) ;
#14508 = CARTESIAN_POINT ( 'NONE',  ( 14.71815190947063812, -2.961536556857895075, -225.5177375088865404 ) ) ;
#14509 = AXIS2_PLACEMENT_3D ( 'NONE', #12815, #9550, #3829 ) ;
#14510 =( BOUNDED_SURFACE ( )  B_SPLINE_SURFACE ( 3, 3, ( 
 ( #20095, #7667, #681, #19574, #2254, #2881, #17684, #14953, #4270, #15060, #4163, #14423, #9877, #8193, #16742, #16108, #1321, #19684, #9354, #15997, #21900, #19359, #17799, #3940, #7555, #10816, #10926, #7449, #14317, #21150, #16214, #5737, #12617, #19461, #2366, #9248, #12841, #21256, #5848, #12729, #11042, #17908, #11149, #2473, #21372, #5965, #9762, #6378, #16627, #8086, #6608, #8532, #6947, #4911, #3555, #10324, #15288, #18976, #193, #16964, #18869, #8419, #22136, #17187, #18656, #3444, #9992, #18543, #13477, #12121, #5240, #3217, #17293, #16853, #6835, #4798, #1764, #8750, #6725, #1541, #10100, #20539, #5021, #13594, #8638, #20316, #10433, #20432, #11896, #20657, #18759, #11790, #3328, #8303, #3110, #15498, #1429, #15169, #22012, #10212, #17079, #1658, #15396, #76, #13357, #1869, #20201, #13819, #22244, #13703, #15612, #5128, #12010, #11673, #19520, #7174, #13931, #5348, #9194, #12563, #19082, #19409, #2091, #10986, #14267, #19307, #2418, #4106, #9302, #3992, #16162, #12460, #8863, #410, #12230, #304, #10541, #5461, #7063, #17855, #21100, #5685, #7398, #628, #8969, #3658, #20766, #10658, #15944, #10869, #14039, #15834, #20875, #16057, #520, #3885, #17411, #1983, #15727, #3776, #7285, #12343, #19196, #17524, #14154, #10765, #7504, #20991, #5581, #17630, #2197, #9078, #17743, #2308, #14371, #21205, #5792, #12672, #8053, #16378, #9848, #957, #14919, #2850, #732, #9517, #9732, #21309, #21760, #841, #11421, #4654, #16267, #18181, #16595, #14592, #13221, #19958, #2637, #6349, #7608, #4318, #6237, #18066, #7831, #14697, #20067, #4429, #11527, #2745, #21531, #2526, #19842, #6122, #7938, #4215, #19737, #4545, #2962, #6015, #7720, #12888, #18397, #14476, #5906, #14801, #12784, #19631, #12994, #21426, #21644, #11311, #9626, #11095, #1177, #16488, #17962, #13111, #11200, #1064, #18291, #9404, #16822, #10181, #20400, #5097, #21980, #16710, #12091, #17049, #15139, #1290, #11866, #3295, #18730, #15367, #15470, #20624, #18946, #6459, #8609, #20285, #21870, #13565, #22213, #1735, #18625, #8504, #6574, #3521, #17159, #4990, #4881, #16934, #13328, #6804, #15030, #11978, #1625, #8164, #1510, #11760, #43, #5208, #13785, #13445, #6915, #13671, #6693, #20170, #4764, #11641, #3187, #18512, #10070, #3077, #1399, #9962, #8272, #8389, #20507, #15257, #22104, #18840, #3413, #10294, #271, #157, #19053, #5315, #10401, #17261, #20843, #1834, #10509, #15694, #7141, #17493, #15579, #14007, #7026, #8712, #13900, #1950, #20735, #5426, #12197, #12309, #17374, #8828, #3628, #19164, #2060, #3739, #10624, #8938, #15805, #12660, #3675, #19726 ),
 ( #11188, #209, #2407, #829, #20782, #4306, #4204, #8880, #12876, #16367, #10559, #12771, #1999, #15744, #323, #18054, #10972, #2623, #9288, #7191, #8767, #4096, #14057, #14464, #10448, #17429, #11083, #9506, #12247, #7078, #19098, #6965, #13836, #21414, #21297, #20673, #12136, #5779, #13947, #5894, #20893, #17842, #5256, #7709, #19506, #18992, #19619, #5363, #16149, #721, #3571, #7595, #17950, #2514, #9392, #16254, #17308, #1884, #14578, #6004, #15628, #18387, #9837, #2950, #21859, #21970, #4872, #18617, #12983, #15131, #4535, #6112, #20057, #6448, #8264, #2841, #15019, #13100, #10062, #1389, #11517, #11411, #1166, #19830, #13318, #21520, #18504, #8154, #3178, #8041, #18280, #6563, #11751, #20277, #19946, #13435, #1280, #944, #7821, #9723, #20159, #16585, #14909, #21749, #14686, #4644, #4416, #16699, #6339, #2735, #4752, #13212, #11631, #11300, #3066, #9954, #18171, #6224, #1054, #16813, #9615, #16477, #7927, #14790, #21632, #22094, #15464, #10173, #1827, #8603, #5201, #5419, #17366, #11970, #6684, #150, #15360, #17042, #6796, #19155, #1618, #10395, #20615, #5309, #22207, #16926, #12302, #17255, #13664, #1500, #12084, #3515, #18940, #15570, #15687, #20837, #3733, #13556, #8822, #20500, #20391, #13776, #7018, #1942, #18832, #8704, #5090, #8379, #265, #13892, #3406, #17152, #4984, #20729, #15248, #12191, #19046, #11859, #1729, #10287, #7135, #18724, #14001, #37, #3289, #3622, #6907, #8496, #10501, #12858, #9041, #9371, #21062, #16231, #17594, #2054, #7245, #11059, #593, #20951, #8932, #19701, #807, #21391, #12635, #5539, #19376, #698, #17486, #10615, #2383, #5983, #5650, #16016, #7466, #12747, #15799, #14555, #3849, #5755, #4183, #2161, #7686, #7574, #12528, #377, #16125, #14115, #3957, #14226, #484, #17818, #2271, #10832, #14440, #10729, #12417, #17704, #7359, #17928, #9154, #15907, #14335, #19269, #21168, #21275, #19482, #4070, #10946, #9267, #5866, #19594, #2491, #21836, #13408, #16791, #11166, #4727, #11390, #18258, #18478, #16561, #14882, #3041, #1366, #4392, #18033, #2602, #6426, #9812, #16343, #16675, #21609, #8241, #11496, #1140, #21946, #15109, #6537, #1255, #4287, #9701, #6088, #19922, #9483, #19808, #7800, #2712, #919, #14665, #18364, #2925, #4622, #20137, #6201, #21499, #12964, #7907, #13190, #8130, #11277, #13078, #18146, #13296, #20034, #8018, #9595, #16458, #1032, #14768, #4509, #2822, #21723, #6316, #14997, #11607, #9927, #8468, #22067, #3154, #7108, #13639, #8575, #4956, #11942, #17229, #15440, #3596, #5282, #20474, #20251, #5066, #12163, #124, #4846, #6770, #6992, #18592, #19019, #20365 ),
 ( #3377, #10258, #13864, #10039, #17016, #10473, #11834, #16899, #18700, #17336, #1915, #3263, #8797, #1475, #13750, #11722, #3490, #15658, #18807, #1592, #10147, #5174, #17125, #1702, #10366, #13524, #238, #15335, #22181, #8351, #10, #6879, #20588, #15222, #6656, #1802, #12056, #18913, #8678, #15542, #20704, #10807, #455, #9241, #778, #4154, #20812, #14416, #21037, #5625, #5840, #3932, #2244, #12720, #11034, #14084, #5388, #12272, #16101, #19453, #3705, #4040, #9013, #17901, #21142, #17673, #9347, #2464, #16207, #10919, #13972, #19350, #15772, #7332, #19125, #7219, #17457, #12390, #10587, #2026, #5729, #12609, #14309, #7548, #15878, #8906, #350, #17567, #565, #17791, #20922, #14200, #5511, #672, #7441, #9126, #19240, #3820, #10703, #2136, #12503, #15988, #2356, #21248, #19567, #11363, #8103, #18120, #9457, #12833, #16762, #1006, #18232, #14640, #21583, #4593, #2792, #13269, #14969, #7881, #7658, #14743, #21810, #9781, #14530, #16431, #16646, #5956, #6398, #7770, #18337, #13048, #6171, #2687, #20112, #18449, #4700, #4365, #11576, #7988, #19896, #19676, #3014, #9898, #6064, #21364, #9569, #4263, #21472, #11141, #18009, #2574, #4484, #16318, #894, #12938, #19784, #11249, #9675, #16534, #1113, #20007, #14852, #21697, #6288, #13162, #11469, #2898, #1229, #3466, #21920, #5261, #16874, #18783, #17207, #15193, #13842, #20563, #3237, #6970, #10453, #4933, #6855, #18676, #10121, #16986, #20679, #5040, #12141, #3349, #1565, #3130, #20451, #8440, #8553, #4819, #20337, #5149, #3576, #6629, #1450, #13499, #18997, #1340, #15517, #15417, #8212, #6510, #22157, #8323, #22260, #15309, #11917, #15084, #1781, #6746, #13380, #13723, #22037, #11809, #13614, #20222, #10232, #17100, #1679, #12031, #18891, #11696, #18565, #10344, #8656, #10010, #100, #3910, #12483, #15967, #16080, #21227, #12696, #7085, #9217, #20900, #216, #14177, #541, #2332, #19218, #9101, #7197, #4130, #17767, #5602, #5485, #17547, #13952, #7419, #15636, #12586, #2220, #19542, #19431, #14288, #20788, #21121, #12368, #5817, #5709, #7307, #17314, #7527, #1890, #4016, #8773, #433, #19103, #10683, #5368, #10564, #12252, #15750, #3680, #14395, #10892, #649, #17653, #17435, #3799, #2004, #8886, #2114, #10786, #329, #14063, #8993, #15856, #21014, #19330, #7854, #7632, #9324, #1200, #7743, #11224, #21335, #21783, #16291, #13243, #14720, #11444, #21449, #12808, #16184, #20087, #4339, #21556, #17985, #2659, #7960, #6146, #16619, #18312, #18091, #11011, #9541, #2872, #13135, #17879, #19759, #19981, #755, #9754, #11117, #21670, #16403, #14615, #8077, #2547, #14501, #9430, #14943 ),
 ( #866, #6370, #14826, #12913, #2441, #5929, #6038, #16509, #979, #13021, #19868, #19652, #4453, #4237, #11335, #18206, #2767, #9648, #1086, #6261, #4568, #1420, #1649, #6939, #9984, #4788, #16845, #1756, #10316, #18860, #18750, #13809, #9868, #3209, #20193, #11888, #18648, #15279, #66, #17179, #4674, #8524, #11549, #10091, #6481, #20306, #16733, #11663, #8185, #3101, #18421, #8630, #3320, #10203, #5012, #20530, #22004, #1312, #2985, #8294, #13586, #17070, #18533, #6599, #15161, #13693, #20423, #1533, #15052, #21892, #15490, #13467, #4903, #13350, #11782, #16956, #8411, #22128, #5119, #6716, #15388, #22236, #6826, #12001, #3435, #5340, #12335, #17623, #15826, #3986, #5678, #14031, #7497, #20867, #12556, #514, #20649, #7165, #7390, #18969, #19403, #20758, #9070, #3765, #17401, #10861, #12222, #3547, #19074, #17737, #2302, #3649, #9186, #17285, #14147, #12113, #3877, #16049, #5452, #1974, #10533, #5572, #19188, #10649, #10758, #13923, #620, #8852, #15719, #5232, #17516, #296, #2084, #15605, #10424, #2189, #1860, #8740, #183, #7053, #8962, #403, #7277, #15939, #20984, #12450, #19300, #21093, #14259, #21419, #6231, #4311, #2630, #13104, #4539, #14469, #21198, #12665, #16481, #19835, #4100, #4422, #9397, #18283, #21524, #11194, #19513, #11304, #12776, #21303, #4209, #16588, #5900, #7825, #18059, #2739, #19624, #14365, #9726, #14690, #11088, #5786, #9511, #949, #16372, #12987, #19950, #2844, #1169, #10978, #11414, #17955, #17848, #6116, #18175, #21636, #16259, #9619, #2520, #2412, #14794, #1058, #835, #14584, #9294, #7931, #16156, #726, #7601, #7714, #6009, #12881, #19731, #19130, #5393, #4755, #15662, #8683, #20593, #13215, #12278, #10593, #6451, #7112, #18811, #13976, #15022, #21752, #4647, #8801, #5179, #18390, #6342, #17462, #20816, #3710, #10371, #2954, #17131, #20709, #14913, #8046, #128, #20060, #3382, #13754, #12061, #10477, #11521, #9842, #1283, #3495, #1920, #21862, #16703, #5287, #10263, #8157, #13321, #11947, #13868, #1707, #8581, #15445, #20162, #18919, #15, #17235, #6885, #1806, #15549, #6996, #12167, #19023, #3601, #17342, #243, #7338, #2141, #14205, #21368, #7664, #16211, #16105, #4267, #7224, #570, #17572, #9245, #15994, #12613, #12837, #2469, #19355, #15883, #14089, #9018, #783, #14534, #21041, #5960, #20929, #17795, #15777, #7552, #19681, #17679, #5631, #12508, #677, #7446, #2251, #14420, #461, #11145, #3937, #10812, #9351, #9131, #14314, #21146, #19246, #5516, #5845, #12395, #3826, #10708, #5734, #19458, #4046, #10923, #19571, #2032, #8911, #356, #2361, #21253, #12724, #4158, #11039 ),
 ( #17905, #21925, #2903, #7994, #13384, #8217, #20228, #14974, #4823, #1118, #19787, #11368, #898, #11254, #21476, #16435, #18013, #15089, #9788, #16653, #18342, #11582, #13056, #7775, #2579, #21588, #4598, #1234, #18124, #19901, #2691, #4705, #11474, #14859, #14645, #16322, #6514, #14747, #18237, #6070, #9462, #1010, #12942, #21702, #18456, #6177, #4370, #9573, #7885, #2797, #6293, #4489, #9680, #21815, #13167, #1346, #3019, #16539, #20012, #8108, #9904, #20116, #6404, #13274, #16767, #10015, #3580, #11813, #104, #17104, #8445, #1894, #19001, #13618, #3470, #1572, #20792, #12145, #22264, #15314, #11921, #16879, #10348, #1454, #6975, #18895, #7089, #18787, #6750, #17318, #220, #8779, #22161, #10457, #12035, #1683, #8327, #15640, #13956, #10126, #11700, #20456, #18570, #18680, #3134, #15197, #22044, #8557, #6633, #13504, #20341, #4937, #3242, #13727, #16991, #5044, #1785, #3355, #10237, #17211, #15421, #6859, #20567, #5155, #13846, #8660, #15521, #20683, #5265, #21231, #19223, #17883, #2337, #7311, #11015, #14505, #8997, #10896, #437, #14182, #21019, #2445, #9105, #9328, #546, #5606, #7201, #2224, #12487, #12590, #8890, #2118, #9221, #7636, #10687, #5489, #17551, #16188, #760, #19546, #19435, #5372, #10569, #3914, #20903, #4020, #19334, #15972, #12256, #5821, #10790, #17439, #17771, #3803, #12373, #15860, #19107, #17657, #21125, #7423, #16084, #14292, #3684, #2008, #5713, #653, #15754, #7531, #14399, #12700, #4136, #333, #14067, #16738, #11121, #13246, #2663, #4241, #18210, #19985, #9547, #17989, #2771, #4572, #6374, #984, #13141, #11227, #8189, #21787, #9652, #16408, #21560, #2551, #11448, #19656, #16623, #6265, #1316, #6150, #7858, #4678, #9872, #18425, #18096, #20091, #21674, #11340, #9435, #2989, #21339, #19763, #11553, #14724, #5934, #6042, #12812, #16295, #870, #16513, #7749, #14619, #21453, #12917, #4343, #1090, #13025, #19872, #18316, #4458, #7964, #2876, #14830, #9758, #1204, #8081, #14949, #13354, #18972, #8299, #10207, #8634, #6603, #5236, #12005, #16960, #20653, #1864, #18652, #20534, #10096, #1537, #8415, #12117, #18755, #3551, #17074, #15283, #16849, #11892, #22132, #22240, #18539, #11786, #18864, #17289, #20311, #15165, #4907, #10428, #15056, #6943, #6831, #21896, #20197, #13590, #22007, #13699, #6720, #3324, #6484, #15494, #20428, #4792, #5124, #13471, #3213, #5017, #11667, #1654, #8528, #15392, #3440, #10320, #3105, #9988, #17183, #1760, #1425, #71, #13814, #3882, #7394, #7501, #12670, #4104, #20762, #625, #20988, #13927, #19518, #10982, #7170, #14369, #19192, #21203, #15723, #188, #5344, #9190 ),
 ( #300, #12226, #8859, #5790, #17853, #14035, #8745, #19078, #2194, #7059, #14264, #15609, #2088, #12339, #20871, #15942, #407, #8966, #21097, #1978, #3653, #3769, #5456, #16054, #15831, #10655, #7281, #10537, #17406, #12561, #17521, #14151, #5576, #12456, #19304, #10762, #17627, #3990, #9074, #518, #5682, #19407, #10866, #17741, #2306, #14694, #12991, #16593, #14917, #2524, #9298, #730, #4543, #7935, #14474, #14799, #19735, #6347, #9623, #21529, #20064, #21756, #4651, #21641, #11525, #7829, #4213, #18063, #7606, #17959, #5904, #839, #2416, #13219, #16485, #1062, #2743, #18287, #4315, #21307, #16160, #6013, #11309, #6235, #9401, #11198, #16265, #11419, #18179, #6119, #12780, #19629, #11092, #21424, #2635, #7718, #14588, #12885, #9515, #19840, #2848, #16375, #954, #4426, #13108, #19955, #9730, #1175, #8050, #9959, #16931, #13325, #8161, #22210, #21866, #1287, #6456, #20167, #15136, #15254, #4877, #13668, #5204, #8606, #2960, #18836, #3183, #10067, #10290, #8386, #6688, #17156, #15466, #18509, #9846, #16707, #20503, #1622, #15027, #8499, #13442, #40, #3292, #22100, #13782, #6911, #20621, #15364, #18395, #1506, #4761, #11756, #11638, #3071, #16818, #1395, #8269, #21977, #10177, #17046, #18727, #11975, #20282, #6571, #18622, #13562, #4987, #6800, #20396, #11862, #5094, #3410, #1732, #8935, #8708, #10398, #2276, #8825, #12305, #154, #596, #17371, #14338, #15802, #12531, #268, #13895, #17258, #21171, #5423, #380, #19050, #3736, #9044, #7248, #17708, #19379, #19160, #12087, #10620, #3960, #14231, #18943, #20840, #21066, #1830, #10835, #12194, #490, #17489, #15690, #9159, #3625, #15575, #10504, #16021, #7469, #1946, #3518, #7023, #5543, #20732, #17597, #5312, #2057, #7138, #14004, #19273, #14119, #20955, #2164, #12422, #3852, #10732, #15910, #7363, #5654, #4075, #7910, #11281, #17823, #18151, #810, #9705, #12967, #18037, #1145, #18261, #8021, #2716, #14887, #11169, #7577, #21395, #10950, #21278, #9270, #4186, #5758, #2825, #19812, #4396, #6092, #21613, #7691, #2385, #12638, #9374, #14668, #9598, #5871, #14559, #12751, #14773, #21502, #2605, #16128, #701, #16565, #2494, #5987, #14443, #19485, #11062, #19599, #9487, #6204, #16234, #17932, #12861, #19705, #4290, #16349, #923, #7803, #16461, #1036, #11393, #13082, #19927, #4513, #4733, #15228, #10044, #21728, #11610, #1481, #20038, #22073, #1259, #16905, #16794, #6430, #13533, #8134, #4625, #15000, #6663, #20371, #21838, #4963, #11499, #6543, #13193, #11729, #11840, #18482, #13299, #20140, #20255, #9932, #3045, #18597, #16679, #6319, #1369, #8245, #18368, #21950, #15113 ),
 ( #2929, #9816, #13414, #4852, #3160, #8358, #2894, #11464, #11358, #21805, #2460, #18115, #12828, #20003, #7876, #888, #19779, #9343, #18227, #17897, #14848, #4478, #14965, #4360, #14635, #9777, #8098, #16642, #16313, #4588, #19890, #9564, #16202, #1224, #6393, #18004, #18333, #7765, #19563, #4258, #11030, #773, #4150, #16426, #7653, #14524, #21359, #5951, #19671, #21578, #11136, #6059, #9670, #2568, #9452, #2787, #21467, #12933, #2682, #1001, #21692, #11243, #14738, #6166, #13043, #13157, #16529, #1108, #7983, #6283, #18885, #94, #16869, #18777, #8317, #15187, #22031, #3459, #16980, #10338, #8434, #6622, #15079, #10115, #13492, #20445, #16757, #10006, #10226, #15512, #18560, #13375, #3126, #17202, #1777, #5144, #5034, #13264, #18445, #11803, #6504, #11911, #4927, #1559, #8651, #13718, #20331, #3008, #3343, #11689, #20217, #1446, #20108, #4812, #6740, #15301, #1672, #18670, #4696, #11571, #13608, #3231, #9892, #22151, #17095, #8547, #15411, #12025, #1335, #8207, #21915, #22256, #6849, #20557, #15323, #8786, #1580, #8564, #13627, #228, #113, #17113, #3365, #20801, #20574, #5053, #12044, #8454, #3249, #17326, #17001, #18687, #22169, #6757, #10246, #10355, #2730, #15647, #340, #3692, #20350, #13962, #5162, #18902, #5379, #3477, #1791, #12262, #10576, #20463, #4945, #11821, #7098, #19009, #10134, #3586, #15428, #17447, #20694, #17218, #8896, #2016, #15762, #10463, #13512, #8667, #11929, #6866, #18796, #1691, #13736, #15530, #6981, #13853, #5271, #12152, #1903, #19115, #2234, #19230, #14074, #20912, #9003, #2454, #17557, #9114, #7319, #16196, #16091, #4030, #3810, #5499, #19665, #3921, #7431, #2126, #17998, #12493, #9446, #10906, #7647, #17663, #15867, #12379, #16307, #554, #17780, #14189, #21132, #4144, #2345, #12822, #14518, #14299, #7208, #5719, #21350, #9336, #10693, #15978, #768, #445, #5945, #21026, #17891, #12598, #10798, #4252, #5615, #19340, #19443, #11130, #2561, #9231, #662, #7538, #14407, #21239, #12709, #5831, #19556, #11023, #13037, #8093, #14843, #1103, #6386, #16420, #20212, #4807, #6498, #15072, #14960, #3121, #6054, #21686, #996, #21800, #6277, #11459, #11683, #1330, #18222, #12928, #13259, #21573, #7871, #19884, #10001, #14734, #16637, #4583, #11565, #6160, #882, #18555, #1218, #4472, #7758, #18328, #9771, #2889, #20102, #21910, #14630, #21462, #19774, #13369, #11352, #13151, #19997, #4353, #11238, #2781, #4691, #9665, #18108, #8202, #18440, #16524, #7977, #2676, #3003, #9558, #9886, #16751, #12240, #17089, #11905, #202, #5357, #13940, #13603, #1877, #17195, #6844, #22026, #20775, #19091, #15296 ) ),
 .UNSPECIFIED., .T., .F., .F. ) 
 B_SPLINE_SURFACE_WITH_KNOTS ( ( 4, 3, 4 ),
 ( 4, 2, 2, 2, 2, 2, 2, 2, 2, 2, 2, 2, 2, 2, 2, 2, 2, 2, 2, 2, 2, 2, 2, 2, 2, 2, 2, 2, 2, 2, 2, 2, 2, 2, 2, 2, 2, 2, 2, 2, 2, 2, 2, 2, 2, 2, 2, 2, 2, 2, 2, 2, 2, 2, 2, 2, 2, 2, 2, 2, 2, 2, 2, 2, 2, 2, 2, 2, 2, 2, 2, 2, 2, 2, 2, 2, 2, 2, 2, 2, 2, 2, 2, 2, 2, 2, 2, 2, 2, 2, 2, 2, 2, 2, 2, 2, 2, 2, 2, 2, 2, 2, 2, 2, 2, 2, 2, 2, 2, 2, 2, 2, 2, 2, 2, 2, 2, 2, 2, 2, 2, 2, 2, 2, 2, 2, 2, 2, 2, 2, 2, 2, 2, 2, 2, 2, 2, 2, 2, 2, 2, 2, 2, 2, 2, 2, 2, 2, 2, 2, 2, 2, 2, 2, 2, 2, 2, 2, 2, 2, 2, 2, 2, 2, 2, 2, 2, 2, 2, 4 ),
 ( 0.000000000000000000, 0.5000000000000000000, 1.000000000000000000 ),
 ( 0.4999446919652688059, 0.5028747035357847839, 0.5058047151063008728, 0.5087347266768169618, 0.5116647382473329397, 0.5145947498178489177, 0.5175247613883648956, 0.5204547729588808735, 0.5233847845293969625, 0.5268031313616656774, 0.5285123047777999794, 0.5302214781939342814, 0.5336398250262029963, 0.5353489984423374093, 0.5370581718584717112, 0.5404765186907403152, 0.5438948655230090301, 0.5473132123552777450, 0.5507315591875463490, 0.5541499060198149529, 0.5575682528520836678, 0.5609865996843523828, 0.5644049465166209867, 0.5661141199327552886, 0.5678232933488895906, 0.5712416401811581945, 0.5729508135972924965, 0.5746599870134267984, 0.5780783338456955134, 0.5814966806779642283, 0.5849150275102328322, 0.5883333743425015472, 0.5917517211747702621, 0.5951700680070388660, 0.5985884148393075810, 0.6020067616715762959, 0.6037159350877105979, 0.6054251085038448998, 0.6088434553361135038, 0.6122618021683822187, 0.6139709755845166317, 0.6156801490006509336, 0.6190984958329195376, 0.6225168426651882525, 0.6259351894974569674, 0.6293535363297255714, 0.6327718831619942863, 0.6361902299942630012, 0.6396085768265316052, 0.6430269236588003201, 0.6447360970749347331, 0.6464452704910690350, 0.6498636173233376390, 0.6532819641556063539, 0.6549911375717407669, 0.6567003109878750688, 0.6601186578201436728, 0.6635370046524122767, 0.6669553514846809916, 0.6703736983169497066, 0.6737920451492183105, 0.6772103919814870254, 0.6806287388137557404, 0.6840470856460243443, 0.6857562590621586462, 0.6866108457702257972, 0.6874654324782930592, 0.6908837793105617742, 0.6943021261428303781, 0.6960112995589646800, 0.6977204729750989820, 0.7011388198073676969, 0.7045571666396364119, 0.7079755134719050158, 0.7113938603041736197, 0.7148122071364423347, 0.7182305539687110496, 0.7216489008009796535, 0.7250672476332483685, 0.7267764210493827814, 0.7284855944655170834, 0.7319039412977856873, 0.7353222881300544023, 0.7387406349623231172, 0.7421589817945917211, 0.7455773286268603250, 0.7489956754591290400, 0.7524140222913977549, 0.7558323691236663588, 0.7592507159559350738, 0.7626690627882037887, 0.7660874096204723926, 0.7695057564527411076, 0.7729241032850098225, 0.7763424501172784264, 0.7797607969495471414, 0.7831791437818158563, 0.7865974906140844602, 0.7900158374463531752, 0.7934341842786218901, 0.7968525311108904940, 0.8002708779431590980, 0.8036892247754278129, 0.8053983981915622259, 0.8071075716076965278, 0.8105259184399651318, 0.8122350918560994337, 0.8139442652722337357, 0.8173626121045024506, 0.8207809589367711656, 0.8241993057690397695, 0.8276176526013083734, 0.8310359994335770883, 0.8344543462658458033, 0.8378726930981144072, 0.8412910399303831221, 0.8430002133465175351, 0.8447093867626518371, 0.8481277335949204410, 0.8515460804271891559, 0.8549644272594578709, 0.8583827740917264748, 0.8618011209239951897, 0.8652194677562639047, 0.8686378145885325086, 0.8720561614208012235, 0.8754745082530699385, 0.8788928550853385424, 0.8823112019176071463, 0.8857295487498758613, 0.8874387221660102743, 0.8891478955821445762, 0.8925662424144131801, 0.8942754158305474821, 0.8959845892466818951, 0.8994029360789506100, 0.9028212829112192139, 0.9062396297434879289, 0.9096579765757566438, 0.9130763234080252477, 0.9164946702402939627, 0.9199130170725626776, 0.9233313639048312815, 0.9250405373209655835, 0.9267497107370999965, 0.9301680575693687114, 0.9335864044016373153, 0.9352955778177716173, 0.9370047512339059192, 0.9404230980661746342, 0.9438414448984433491, 0.9472597917307119531, 0.9506781385629806680, 0.9540964853952493829, 0.9575148322275179869, 0.9609331790597867018, 0.9643515258920554167, 0.9660606993081897187, 0.9677698727243240207, 0.9711882195565927356, 0.9728973929727271486, 0.9746065663888614505, 0.9780249132211300545, 0.9814432600533987694, 0.9848616068856674843, 0.9882799537179360883, 0.9912099652884520662, 0.9941399768589680441, 0.9970699884294840221, 1.000000000000000000 ),
 .UNSPECIFIED. ) 
 GEOMETRIC_REPRESENTATION_ITEM ( )  RATIONAL_B_SPLINE_SURFACE ( (
 ( 1.000000000000000000, 1.000000000000000000, 1.000000000000000000, 1.000000000000000000, 1.000000000000000000, 1.000000000000000000, 1.000000000000000000, 1.000000000000000000, 1.000000000000000000, 1.000000000000000000, 1.000000000000000000, 1.000000000000000000, 1.000000000000000000, 1.000000000000000000, 1.000000000000000000, 1.000000000000000000, 1.000000000000000000, 1.000000000000000000, 1.000000000000000000, 1.000000000000000000, 1.000000000000000000, 1.000000000000000000, 1.000000000000000000, 1.000000000000000000, 1.000000000000000000, 1.000000000000000000, 1.000000000000000000, 1.000000000000000000, 1.000000000000000000, 1.000000000000000000, 1.000000000000000000, 1.000000000000000000, 1.000000000000000000, 1.000000000000000000, 1.000000000000000000, 1.000000000000000000, 1.000000000000000000, 1.000000000000000000, 1.000000000000000000, 1.000000000000000000, 1.000000000000000000, 1.000000000000000000, 1.000000000000000000, 1.000000000000000000, 1.000000000000000000, 1.000000000000000000, 1.000000000000000000, 1.000000000000000000, 1.000000000000000000, 1.000000000000000000, 1.000000000000000000, 1.000000000000000000, 1.000000000000000000, 1.000000000000000000, 1.000000000000000000, 1.000000000000000000, 1.000000000000000000, 1.000000000000000000, 1.000000000000000000, 1.000000000000000000, 1.000000000000000000, 1.000000000000000000, 1.000000000000000000, 1.000000000000000000, 1.000000000000000000, 1.000000000000000000, 1.000000000000000000, 1.000000000000000000, 1.000000000000000000, 1.000000000000000000, 1.000000000000000000, 1.000000000000000000, 1.000000000000000000, 1.000000000000000000, 1.000000000000000000, 1.000000000000000000, 1.000000000000000000, 1.000000000000000000, 1.000000000000000000, 1.000000000000000000, 1.000000000000000000, 1.000000000000000000, 1.000000000000000000, 1.000000000000000000, 1.000000000000000000, 1.000000000000000000, 1.000000000000000000, 1.000000000000000000, 1.000000000000000000, 1.000000000000000000, 1.000000000000000000, 1.000000000000000000, 1.000000000000000000, 1.000000000000000000, 1.000000000000000000, 1.000000000000000000, 1.000000000000000000, 1.000000000000000000, 1.000000000000000000, 1.000000000000000000, 1.000000000000000000, 1.000000000000000000, 1.000000000000000000, 1.000000000000000000, 1.000000000000000000, 1.000000000000000000, 1.000000000000000000, 1.000000000000000000, 1.000000000000000000, 1.000000000000000000, 1.000000000000000000, 1.000000000000000000, 1.000000000000000000, 1.000000000000000000, 1.000000000000000000, 1.000000000000000000, 1.000000000000000000, 1.000000000000000000, 1.000000000000000000, 1.000000000000000000, 1.000000000000000000, 1.000000000000000000, 1.000000000000000000, 1.000000000000000000, 1.000000000000000000, 1.000000000000000000, 1.000000000000000000, 1.000000000000000000, 1.000000000000000000, 1.000000000000000000, 1.000000000000000000, 1.000000000000000000, 1.000000000000000000, 1.000000000000000000, 1.000000000000000000, 1.000000000000000000, 1.000000000000000000, 1.000000000000000000, 1.000000000000000000, 1.000000000000000000, 1.000000000000000000, 1.000000000000000000, 1.000000000000000000, 1.000000000000000000, 1.000000000000000000, 1.000000000000000000, 1.000000000000000000, 1.000000000000000000, 1.000000000000000000, 1.000000000000000000, 1.000000000000000000, 1.000000000000000000, 1.000000000000000000, 1.000000000000000000, 1.000000000000000000, 1.000000000000000000, 1.000000000000000000, 1.000000000000000000, 1.000000000000000000, 1.000000000000000000, 1.000000000000000000, 1.000000000000000000, 1.000000000000000000, 1.000000000000000000, 1.000000000000000000, 1.000000000000000000, 1.000000000000000000, 1.000000000000000000, 1.000000000000000000, 1.000000000000000000, 1.000000000000000000, 1.000000000000000000, 1.000000000000000000, 1.000000000000000000, 1.000000000000000000, 1.000000000000000000, 1.000000000000000000, 1.000000000000000000, 1.000000000000000000, 1.000000000000000000, 1.000000000000000000, 1.000000000000000000, 1.000000000000000000, 1.000000000000000000, 1.000000000000000000, 1.000000000000000000, 1.000000000000000000, 1.000000000000000000, 1.000000000000000000, 1.000000000000000000, 1.000000000000000000, 1.000000000000000000, 1.000000000000000000, 1.000000000000000000, 1.000000000000000000, 1.000000000000000000, 1.000000000000000000, 1.000000000000000000, 1.000000000000000000, 1.000000000000000000, 1.000000000000000000, 1.000000000000000000, 1.000000000000000000, 1.000000000000000000, 1.000000000000000000, 1.000000000000000000, 1.000000000000000000, 1.000000000000000000, 1.000000000000000000, 1.000000000000000000, 1.000000000000000000, 1.000000000000000000, 1.000000000000000000, 1.000000000000000000, 1.000000000000000000, 1.000000000000000000, 1.000000000000000000, 1.000000000000000000, 1.000000000000000000, 1.000000000000000000, 1.000000000000000000, 1.000000000000000000, 1.000000000000000000, 1.000000000000000000, 1.000000000000000000, 1.000000000000000000, 1.000000000000000000, 1.000000000000000000, 1.000000000000000000, 1.000000000000000000, 1.000000000000000000, 1.000000000000000000, 1.000000000000000000, 1.000000000000000000, 1.000000000000000000, 1.000000000000000000, 1.000000000000000000, 1.000000000000000000, 1.000000000000000000, 1.000000000000000000, 1.000000000000000000, 1.000000000000000000, 1.000000000000000000, 1.000000000000000000, 1.000000000000000000, 1.000000000000000000, 1.000000000000000000, 1.000000000000000000, 1.000000000000000000, 1.000000000000000000, 1.000000000000000000, 1.000000000000000000, 1.000000000000000000, 1.000000000000000000, 1.000000000000000000, 1.000000000000000000, 1.000000000000000000, 1.000000000000000000, 1.000000000000000000, 1.000000000000000000, 1.000000000000000000, 1.000000000000000000, 1.000000000000000000, 1.000000000000000000, 1.000000000000000000, 1.000000000000000000, 1.000000000000000000, 1.000000000000000000, 1.000000000000000000, 1.000000000000000000, 1.000000000000000000, 1.000000000000000000, 1.000000000000000000, 1.000000000000000000, 1.000000000000000000, 1.000000000000000000, 1.000000000000000000, 1.000000000000000000, 1.000000000000000000, 1.000000000000000000, 1.000000000000000000, 1.000000000000000000, 1.000000000000000000, 1.000000000000000000, 1.000000000000000000, 1.000000000000000000, 1.000000000000000000, 1.000000000000000000, 1.000000000000000000, 1.000000000000000000, 1.000000000000000000, 1.000000000000000000, 1.000000000000000000, 1.000000000000000000, 1.000000000000000000, 1.000000000000000000, 1.000000000000000000, 1.000000000000000000, 1.000000000000000000, 1.000000000000000000, 1.000000000000000000, 1.000000000000000000, 1.000000000000000000, 1.000000000000000000, 1.000000000000000000, 1.000000000000000000, 1.000000000000000000, 1.000000000000000000, 1.000000000000000000, 1.000000000000000000, 1.000000000000000000, 1.000000000000000000, 1.000000000000000000, 1.000000000000000000, 1.000000000000000000, 1.000000000000000000, 1.000000000000000000, 1.000000000000000000, 1.000000000000000000, 1.000000000000000000, 1.000000000000000000, 1.000000000000000000, 1.000000000000000000, 1.000000000000000000, 1.000000000000000000, 1.000000000000000000, 1.000000000000000000, 1.000000000000000000, 1.000000000000000000, 1.000000000000000000, 1.000000000000000000, 1.000000000000000000, 1.000000000000000000, 1.000000000000000000, 1.000000000000000000, 1.000000000000000000, 1.000000000000000000, 1.000000000000000000, 1.000000000000000000, 1.000000000000000000),
 ( 0.3333333333333333703, 0.3333333333333333703, 0.3333333333333333703, 0.3333333333333333703, 0.3333333333333333703, 0.3333333333333333703, 0.3333333333333333703, 0.3333333333333333703, 0.3333333333333333703, 0.3333333333333333703, 0.3333333333333333703, 0.3333333333333333703, 0.3333333333333333703, 0.3333333333333333703, 0.3333333333333333703, 0.3333333333333333703, 0.3333333333333333703, 0.3333333333333333703, 0.3333333333333333703, 0.3333333333333333703, 0.3333333333333333703, 0.3333333333333333703, 0.3333333333333333703, 0.3333333333333333703, 0.3333333333333333703, 0.3333333333333333703, 0.3333333333333333703, 0.3333333333333333703, 0.3333333333333333703, 0.3333333333333333703, 0.3333333333333333703, 0.3333333333333333703, 0.3333333333333333703, 0.3333333333333333703, 0.3333333333333333703, 0.3333333333333333703, 0.3333333333333333703, 0.3333333333333333703, 0.3333333333333333703, 0.3333333333333333703, 0.3333333333333333703, 0.3333333333333333703, 0.3333333333333333703, 0.3333333333333333703, 0.3333333333333333703, 0.3333333333333333703, 0.3333333333333333703, 0.3333333333333333703, 0.3333333333333333703, 0.3333333333333333703, 0.3333333333333333703, 0.3333333333333333703, 0.3333333333333333703, 0.3333333333333333703, 0.3333333333333333703, 0.3333333333333333703, 0.3333333333333333703, 0.3333333333333333703, 0.3333333333333333703, 0.3333333333333333703, 0.3333333333333333703, 0.3333333333333333703, 0.3333333333333333703, 0.3333333333333333703, 0.3333333333333333703, 0.3333333333333333703, 0.3333333333333333703, 0.3333333333333333703, 0.3333333333333333703, 0.3333333333333333703, 0.3333333333333333703, 0.3333333333333333703, 0.3333333333333333703, 0.3333333333333333703, 0.3333333333333333703, 0.3333333333333333703, 0.3333333333333333703, 0.3333333333333333703, 0.3333333333333333703, 0.3333333333333333703, 0.3333333333333333703, 0.3333333333333333703, 0.3333333333333333703, 0.3333333333333333703, 0.3333333333333333703, 0.3333333333333333703, 0.3333333333333333703, 0.3333333333333333703, 0.3333333333333333703, 0.3333333333333333703, 0.3333333333333333703, 0.3333333333333333703, 0.3333333333333333703, 0.3333333333333333703, 0.3333333333333333703, 0.3333333333333333703, 0.3333333333333333703, 0.3333333333333333703, 0.3333333333333333703, 0.3333333333333333703, 0.3333333333333333703, 0.3333333333333333703, 0.3333333333333333703, 0.3333333333333333703, 0.3333333333333333703, 0.3333333333333333703, 0.3333333333333333703, 0.3333333333333333703, 0.3333333333333333703, 0.3333333333333333703, 0.3333333333333333703, 0.3333333333333333703, 0.3333333333333333703, 0.3333333333333333703, 0.3333333333333333703, 0.3333333333333333703, 0.3333333333333333703, 0.3333333333333333703, 0.3333333333333333703, 0.3333333333333333703, 0.3333333333333333703, 0.3333333333333333703, 0.3333333333333333703, 0.3333333333333333703, 0.3333333333333333703, 0.3333333333333333703, 0.3333333333333333703, 0.3333333333333333703, 0.3333333333333333703, 0.3333333333333333703, 0.3333333333333333703, 0.3333333333333333703, 0.3333333333333333703, 0.3333333333333333703, 0.3333333333333333703, 0.3333333333333333703, 0.3333333333333333703, 0.3333333333333333703, 0.3333333333333333703, 0.3333333333333333703, 0.3333333333333333703, 0.3333333333333333703, 0.3333333333333333703, 0.3333333333333333703, 0.3333333333333333703, 0.3333333333333333703, 0.3333333333333333703, 0.3333333333333333703, 0.3333333333333333703, 0.3333333333333333703, 0.3333333333333333703, 0.3333333333333333703, 0.3333333333333333703, 0.3333333333333333703, 0.3333333333333333703, 0.3333333333333333703, 0.3333333333333333703, 0.3333333333333333703, 0.3333333333333333703, 0.3333333333333333703, 0.3333333333333333703, 0.3333333333333333703, 0.3333333333333333703, 0.3333333333333333703, 0.3333333333333333703, 0.3333333333333333703, 0.3333333333333333703, 0.3333333333333333703, 0.3333333333333333703, 0.3333333333333333703, 0.3333333333333333703, 0.3333333333333333703, 0.3333333333333333703, 0.3333333333333333703, 0.3333333333333333703, 0.3333333333333333703, 0.3333333333333333703, 0.3333333333333333703, 0.3333333333333333703, 0.3333333333333333703, 0.3333333333333333703, 0.3333333333333333703, 0.3333333333333333703, 0.3333333333333333703, 0.3333333333333333703, 0.3333333333333333703, 0.3333333333333333703, 0.3333333333333333703, 0.3333333333333333703, 0.3333333333333333703, 0.3333333333333333703, 0.3333333333333333703, 0.3333333333333333703, 0.3333333333333333703, 0.3333333333333333703, 0.3333333333333333703, 0.3333333333333333703, 0.3333333333333333703, 0.3333333333333333703, 0.3333333333333333703, 0.3333333333333333703, 0.3333333333333333703, 0.3333333333333333703, 0.3333333333333333703, 0.3333333333333333703, 0.3333333333333333703, 0.3333333333333333703, 0.3333333333333333703, 0.3333333333333333703, 0.3333333333333333703, 0.3333333333333333703, 0.3333333333333333703, 0.3333333333333333703, 0.3333333333333333703, 0.3333333333333333703, 0.3333333333333333703, 0.3333333333333333703, 0.3333333333333333703, 0.3333333333333333703, 0.3333333333333333703, 0.3333333333333333703, 0.3333333333333333703, 0.3333333333333333703, 0.3333333333333333703, 0.3333333333333333703, 0.3333333333333333703, 0.3333333333333333703, 0.3333333333333333703, 0.3333333333333333703, 0.3333333333333333703, 0.3333333333333333703, 0.3333333333333333703, 0.3333333333333333703, 0.3333333333333333703, 0.3333333333333333703, 0.3333333333333333703, 0.3333333333333333703, 0.3333333333333333703, 0.3333333333333333703, 0.3333333333333333703, 0.3333333333333333703, 0.3333333333333333703, 0.3333333333333333703, 0.3333333333333333703, 0.3333333333333333703, 0.3333333333333333703, 0.3333333333333333703, 0.3333333333333333703, 0.3333333333333333703, 0.3333333333333333703, 0.3333333333333333703, 0.3333333333333333703, 0.3333333333333333703, 0.3333333333333333703, 0.3333333333333333703, 0.3333333333333333703, 0.3333333333333333703, 0.3333333333333333703, 0.3333333333333333703, 0.3333333333333333703, 0.3333333333333333703, 0.3333333333333333703, 0.3333333333333333703, 0.3333333333333333703, 0.3333333333333333703, 0.3333333333333333703, 0.3333333333333333703, 0.3333333333333333703, 0.3333333333333333703, 0.3333333333333333703, 0.3333333333333333703, 0.3333333333333333703, 0.3333333333333333703, 0.3333333333333333703, 0.3333333333333333703, 0.3333333333333333703, 0.3333333333333333703, 0.3333333333333333703, 0.3333333333333333703, 0.3333333333333333703, 0.3333333333333333703, 0.3333333333333333703, 0.3333333333333333703, 0.3333333333333333703, 0.3333333333333333703, 0.3333333333333333703, 0.3333333333333333703, 0.3333333333333333703, 0.3333333333333333703, 0.3333333333333333703, 0.3333333333333333703, 0.3333333333333333703, 0.3333333333333333703, 0.3333333333333333703, 0.3333333333333333703, 0.3333333333333333703, 0.3333333333333333703, 0.3333333333333333703, 0.3333333333333333703, 0.3333333333333333703, 0.3333333333333333703, 0.3333333333333333703, 0.3333333333333333703, 0.3333333333333333703, 0.3333333333333333703, 0.3333333333333333703, 0.3333333333333333703, 0.3333333333333333703, 0.3333333333333333703, 0.3333333333333333703, 0.3333333333333333703, 0.3333333333333333703, 0.3333333333333333703, 0.3333333333333333703, 0.3333333333333333703, 0.3333333333333333703, 0.3333333333333333703, 0.3333333333333333703, 0.3333333333333333703, 0.3333333333333333703, 0.3333333333333333703, 0.3333333333333333703, 0.3333333333333333703, 0.3333333333333333703, 0.3333333333333333703, 0.3333333333333333703, 0.3333333333333333703, 0.3333333333333333703, 0.3333333333333333703, 0.3333333333333333703, 0.3333333333333333703, 0.3333333333333333703, 0.3333333333333333703, 0.3333333333333333703, 0.3333333333333333703, 0.3333333333333333703, 0.3333333333333333703, 0.3333333333333333703, 0.3333333333333333703, 0.3333333333333333703),
 ( 0.3333333333333333703, 0.3333333333333333703, 0.3333333333333333703, 0.3333333333333333703, 0.3333333333333333703, 0.3333333333333333703, 0.3333333333333333703, 0.3333333333333333703, 0.3333333333333333703, 0.3333333333333333703, 0.3333333333333333703, 0.3333333333333333703, 0.3333333333333333703, 0.3333333333333333703, 0.3333333333333333703, 0.3333333333333333703, 0.3333333333333333703, 0.3333333333333333703, 0.3333333333333333703, 0.3333333333333333703, 0.3333333333333333703, 0.3333333333333333703, 0.3333333333333333703, 0.3333333333333333703, 0.3333333333333333703, 0.3333333333333333703, 0.3333333333333333703, 0.3333333333333333703, 0.3333333333333333703, 0.3333333333333333703, 0.3333333333333333703, 0.3333333333333333703, 0.3333333333333333703, 0.3333333333333333703, 0.3333333333333333703, 0.3333333333333333703, 0.3333333333333333703, 0.3333333333333333703, 0.3333333333333333703, 0.3333333333333333703, 0.3333333333333333703, 0.3333333333333333703, 0.3333333333333333703, 0.3333333333333333703, 0.3333333333333333703, 0.3333333333333333703, 0.3333333333333333703, 0.3333333333333333703, 0.3333333333333333703, 0.3333333333333333703, 0.3333333333333333703, 0.3333333333333333703, 0.3333333333333333703, 0.3333333333333333703, 0.3333333333333333703, 0.3333333333333333703, 0.3333333333333333703, 0.3333333333333333703, 0.3333333333333333703, 0.3333333333333333703, 0.3333333333333333703, 0.3333333333333333703, 0.3333333333333333703, 0.3333333333333333703, 0.3333333333333333703, 0.3333333333333333703, 0.3333333333333333703, 0.3333333333333333703, 0.3333333333333333703, 0.3333333333333333703, 0.3333333333333333703, 0.3333333333333333703, 0.3333333333333333703, 0.3333333333333333703, 0.3333333333333333703, 0.3333333333333333703, 0.3333333333333333703, 0.3333333333333333703, 0.3333333333333333703, 0.3333333333333333703, 0.3333333333333333703, 0.3333333333333333703, 0.3333333333333333703, 0.3333333333333333703, 0.3333333333333333703, 0.3333333333333333703, 0.3333333333333333703, 0.3333333333333333703, 0.3333333333333333703, 0.3333333333333333703, 0.3333333333333333703, 0.3333333333333333703, 0.3333333333333333703, 0.3333333333333333703, 0.3333333333333333703, 0.3333333333333333703, 0.3333333333333333703, 0.3333333333333333703, 0.3333333333333333703, 0.3333333333333333703, 0.3333333333333333703, 0.3333333333333333703, 0.3333333333333333703, 0.3333333333333333703, 0.3333333333333333703, 0.3333333333333333703, 0.3333333333333333703, 0.3333333333333333703, 0.3333333333333333703, 0.3333333333333333703, 0.3333333333333333703, 0.3333333333333333703, 0.3333333333333333703, 0.3333333333333333703, 0.3333333333333333703, 0.3333333333333333703, 0.3333333333333333703, 0.3333333333333333703, 0.3333333333333333703, 0.3333333333333333703, 0.3333333333333333703, 0.3333333333333333703, 0.3333333333333333703, 0.3333333333333333703, 0.3333333333333333703, 0.3333333333333333703, 0.3333333333333333703, 0.3333333333333333703, 0.3333333333333333703, 0.3333333333333333703, 0.3333333333333333703, 0.3333333333333333703, 0.3333333333333333703, 0.3333333333333333703, 0.3333333333333333703, 0.3333333333333333703, 0.3333333333333333703, 0.3333333333333333703, 0.3333333333333333703, 0.3333333333333333703, 0.3333333333333333703, 0.3333333333333333703, 0.3333333333333333703, 0.3333333333333333703, 0.3333333333333333703, 0.3333333333333333703, 0.3333333333333333703, 0.3333333333333333703, 0.3333333333333333703, 0.3333333333333333703, 0.3333333333333333703, 0.3333333333333333703, 0.3333333333333333703, 0.3333333333333333703, 0.3333333333333333703, 0.3333333333333333703, 0.3333333333333333703, 0.3333333333333333703, 0.3333333333333333703, 0.3333333333333333703, 0.3333333333333333703, 0.3333333333333333703, 0.3333333333333333703, 0.3333333333333333703, 0.3333333333333333703, 0.3333333333333333703, 0.3333333333333333703, 0.3333333333333333703, 0.3333333333333333703, 0.3333333333333333703, 0.3333333333333333703, 0.3333333333333333703, 0.3333333333333333703, 0.3333333333333333703, 0.3333333333333333703, 0.3333333333333333703, 0.3333333333333333703, 0.3333333333333333703, 0.3333333333333333703, 0.3333333333333333703, 0.3333333333333333703, 0.3333333333333333703, 0.3333333333333333703, 0.3333333333333333703, 0.3333333333333333703, 0.3333333333333333703, 0.3333333333333333703, 0.3333333333333333703, 0.3333333333333333703, 0.3333333333333333703, 0.3333333333333333703, 0.3333333333333333703, 0.3333333333333333703, 0.3333333333333333703, 0.3333333333333333703, 0.3333333333333333703, 0.3333333333333333703, 0.3333333333333333703, 0.3333333333333333703, 0.3333333333333333703, 0.3333333333333333703, 0.3333333333333333703, 0.3333333333333333703, 0.3333333333333333703, 0.3333333333333333703, 0.3333333333333333703, 0.3333333333333333703, 0.3333333333333333703, 0.3333333333333333703, 0.3333333333333333703, 0.3333333333333333703, 0.3333333333333333703, 0.3333333333333333703, 0.3333333333333333703, 0.3333333333333333703, 0.3333333333333333703, 0.3333333333333333703, 0.3333333333333333703, 0.3333333333333333703, 0.3333333333333333703, 0.3333333333333333703, 0.3333333333333333703, 0.3333333333333333703, 0.3333333333333333703, 0.3333333333333333703, 0.3333333333333333703, 0.3333333333333333703, 0.3333333333333333703, 0.3333333333333333703, 0.3333333333333333703, 0.3333333333333333703, 0.3333333333333333703, 0.3333333333333333703, 0.3333333333333333703, 0.3333333333333333703, 0.3333333333333333703, 0.3333333333333333703, 0.3333333333333333703, 0.3333333333333333703, 0.3333333333333333703, 0.3333333333333333703, 0.3333333333333333703, 0.3333333333333333703, 0.3333333333333333703, 0.3333333333333333703, 0.3333333333333333703, 0.3333333333333333703, 0.3333333333333333703, 0.3333333333333333703, 0.3333333333333333703, 0.3333333333333333703, 0.3333333333333333703, 0.3333333333333333703, 0.3333333333333333703, 0.3333333333333333703, 0.3333333333333333703, 0.3333333333333333703, 0.3333333333333333703, 0.3333333333333333703, 0.3333333333333333703, 0.3333333333333333703, 0.3333333333333333703, 0.3333333333333333703, 0.3333333333333333703, 0.3333333333333333703, 0.3333333333333333703, 0.3333333333333333703, 0.3333333333333333703, 0.3333333333333333703, 0.3333333333333333703, 0.3333333333333333703, 0.3333333333333333703, 0.3333333333333333703, 0.3333333333333333703, 0.3333333333333333703, 0.3333333333333333703, 0.3333333333333333703, 0.3333333333333333703, 0.3333333333333333703, 0.3333333333333333703, 0.3333333333333333703, 0.3333333333333333703, 0.3333333333333333703, 0.3333333333333333703, 0.3333333333333333703, 0.3333333333333333703, 0.3333333333333333703, 0.3333333333333333703, 0.3333333333333333703, 0.3333333333333333703, 0.3333333333333333703, 0.3333333333333333703, 0.3333333333333333703, 0.3333333333333333703, 0.3333333333333333703, 0.3333333333333333703, 0.3333333333333333703, 0.3333333333333333703, 0.3333333333333333703, 0.3333333333333333703, 0.3333333333333333703, 0.3333333333333333703, 0.3333333333333333703, 0.3333333333333333703, 0.3333333333333333703, 0.3333333333333333703, 0.3333333333333333703, 0.3333333333333333703, 0.3333333333333333703, 0.3333333333333333703, 0.3333333333333333703, 0.3333333333333333703, 0.3333333333333333703, 0.3333333333333333703, 0.3333333333333333703, 0.3333333333333333703, 0.3333333333333333703, 0.3333333333333333703, 0.3333333333333333703, 0.3333333333333333703, 0.3333333333333333703, 0.3333333333333333703, 0.3333333333333333703, 0.3333333333333333703, 0.3333333333333333703, 0.3333333333333333703, 0.3333333333333333703, 0.3333333333333333703, 0.3333333333333333703, 0.3333333333333333703, 0.3333333333333333703, 0.3333333333333333703, 0.3333333333333333703, 0.3333333333333333703, 0.3333333333333333703, 0.3333333333333333703, 0.3333333333333333703, 0.3333333333333333703, 0.3333333333333333703, 0.3333333333333333703),
 ( 1.000000000000000000, 1.000000000000000000, 1.000000000000000000, 1.000000000000000000, 1.000000000000000000, 1.000000000000000000, 1.000000000000000000, 1.000000000000000000, 1.000000000000000000, 1.000000000000000000, 1.000000000000000000, 1.000000000000000000, 1.000000000000000000, 1.000000000000000000, 1.000000000000000000, 1.000000000000000000, 1.000000000000000000, 1.000000000000000000, 1.000000000000000000, 1.000000000000000000, 1.000000000000000000, 1.000000000000000000, 1.000000000000000000, 1.000000000000000000, 1.000000000000000000, 1.000000000000000000, 1.000000000000000000, 1.000000000000000000, 1.000000000000000000, 1.000000000000000000, 1.000000000000000000, 1.000000000000000000, 1.000000000000000000, 1.000000000000000000, 1.000000000000000000, 1.000000000000000000, 1.000000000000000000, 1.000000000000000000, 1.000000000000000000, 1.000000000000000000, 1.000000000000000000, 1.000000000000000000, 1.000000000000000000, 1.000000000000000000, 1.000000000000000000, 1.000000000000000000, 1.000000000000000000, 1.000000000000000000, 1.000000000000000000, 1.000000000000000000, 1.000000000000000000, 1.000000000000000000, 1.000000000000000000, 1.000000000000000000, 1.000000000000000000, 1.000000000000000000, 1.000000000000000000, 1.000000000000000000, 1.000000000000000000, 1.000000000000000000, 1.000000000000000000, 1.000000000000000000, 1.000000000000000000, 1.000000000000000000, 1.000000000000000000, 1.000000000000000000, 1.000000000000000000, 1.000000000000000000, 1.000000000000000000, 1.000000000000000000, 1.000000000000000000, 1.000000000000000000, 1.000000000000000000, 1.000000000000000000, 1.000000000000000000, 1.000000000000000000, 1.000000000000000000, 1.000000000000000000, 1.000000000000000000, 1.000000000000000000, 1.000000000000000000, 1.000000000000000000, 1.000000000000000000, 1.000000000000000000, 1.000000000000000000, 1.000000000000000000, 1.000000000000000000, 1.000000000000000000, 1.000000000000000000, 1.000000000000000000, 1.000000000000000000, 1.000000000000000000, 1.000000000000000000, 1.000000000000000000, 1.000000000000000000, 1.000000000000000000, 1.000000000000000000, 1.000000000000000000, 1.000000000000000000, 1.000000000000000000, 1.000000000000000000, 1.000000000000000000, 1.000000000000000000, 1.000000000000000000, 1.000000000000000000, 1.000000000000000000, 1.000000000000000000, 1.000000000000000000, 1.000000000000000000, 1.000000000000000000, 1.000000000000000000, 1.000000000000000000, 1.000000000000000000, 1.000000000000000000, 1.000000000000000000, 1.000000000000000000, 1.000000000000000000, 1.000000000000000000, 1.000000000000000000, 1.000000000000000000, 1.000000000000000000, 1.000000000000000000, 1.000000000000000000, 1.000000000000000000, 1.000000000000000000, 1.000000000000000000, 1.000000000000000000, 1.000000000000000000, 1.000000000000000000, 1.000000000000000000, 1.000000000000000000, 1.000000000000000000, 1.000000000000000000, 1.000000000000000000, 1.000000000000000000, 1.000000000000000000, 1.000000000000000000, 1.000000000000000000, 1.000000000000000000, 1.000000000000000000, 1.000000000000000000, 1.000000000000000000, 1.000000000000000000, 1.000000000000000000, 1.000000000000000000, 1.000000000000000000, 1.000000000000000000, 1.000000000000000000, 1.000000000000000000, 1.000000000000000000, 1.000000000000000000, 1.000000000000000000, 1.000000000000000000, 1.000000000000000000, 1.000000000000000000, 1.000000000000000000, 1.000000000000000000, 1.000000000000000000, 1.000000000000000000, 1.000000000000000000, 1.000000000000000000, 1.000000000000000000, 1.000000000000000000, 1.000000000000000000, 1.000000000000000000, 1.000000000000000000, 1.000000000000000000, 1.000000000000000000, 1.000000000000000000, 1.000000000000000000, 1.000000000000000000, 1.000000000000000000, 1.000000000000000000, 1.000000000000000000, 1.000000000000000000, 1.000000000000000000, 1.000000000000000000, 1.000000000000000000, 1.000000000000000000, 1.000000000000000000, 1.000000000000000000, 1.000000000000000000, 1.000000000000000000, 1.000000000000000000, 1.000000000000000000, 1.000000000000000000, 1.000000000000000000, 1.000000000000000000, 1.000000000000000000, 1.000000000000000000, 1.000000000000000000, 1.000000000000000000, 1.000000000000000000, 1.000000000000000000, 1.000000000000000000, 1.000000000000000000, 1.000000000000000000, 1.000000000000000000, 1.000000000000000000, 1.000000000000000000, 1.000000000000000000, 1.000000000000000000, 1.000000000000000000, 1.000000000000000000, 1.000000000000000000, 1.000000000000000000, 1.000000000000000000, 1.000000000000000000, 1.000000000000000000, 1.000000000000000000, 1.000000000000000000, 1.000000000000000000, 1.000000000000000000, 1.000000000000000000, 1.000000000000000000, 1.000000000000000000, 1.000000000000000000, 1.000000000000000000, 1.000000000000000000, 1.000000000000000000, 1.000000000000000000, 1.000000000000000000, 1.000000000000000000, 1.000000000000000000, 1.000000000000000000, 1.000000000000000000, 1.000000000000000000, 1.000000000000000000, 1.000000000000000000, 1.000000000000000000, 1.000000000000000000, 1.000000000000000000, 1.000000000000000000, 1.000000000000000000, 1.000000000000000000, 1.000000000000000000, 1.000000000000000000, 1.000000000000000000, 1.000000000000000000, 1.000000000000000000, 1.000000000000000000, 1.000000000000000000, 1.000000000000000000, 1.000000000000000000, 1.000000000000000000, 1.000000000000000000, 1.000000000000000000, 1.000000000000000000, 1.000000000000000000, 1.000000000000000000, 1.000000000000000000, 1.000000000000000000, 1.000000000000000000, 1.000000000000000000, 1.000000000000000000, 1.000000000000000000, 1.000000000000000000, 1.000000000000000000, 1.000000000000000000, 1.000000000000000000, 1.000000000000000000, 1.000000000000000000, 1.000000000000000000, 1.000000000000000000, 1.000000000000000000, 1.000000000000000000, 1.000000000000000000, 1.000000000000000000, 1.000000000000000000, 1.000000000000000000, 1.000000000000000000, 1.000000000000000000, 1.000000000000000000, 1.000000000000000000, 1.000000000000000000, 1.000000000000000000, 1.000000000000000000, 1.000000000000000000, 1.000000000000000000, 1.000000000000000000, 1.000000000000000000, 1.000000000000000000, 1.000000000000000000, 1.000000000000000000, 1.000000000000000000, 1.000000000000000000, 1.000000000000000000, 1.000000000000000000, 1.000000000000000000, 1.000000000000000000, 1.000000000000000000, 1.000000000000000000, 1.000000000000000000, 1.000000000000000000, 1.000000000000000000, 1.000000000000000000, 1.000000000000000000, 1.000000000000000000, 1.000000000000000000, 1.000000000000000000, 1.000000000000000000, 1.000000000000000000, 1.000000000000000000, 1.000000000000000000, 1.000000000000000000, 1.000000000000000000, 1.000000000000000000, 1.000000000000000000, 1.000000000000000000, 1.000000000000000000, 1.000000000000000000, 1.000000000000000000, 1.000000000000000000, 1.000000000000000000, 1.000000000000000000, 1.000000000000000000, 1.000000000000000000, 1.000000000000000000, 1.000000000000000000, 1.000000000000000000, 1.000000000000000000, 1.000000000000000000, 1.000000000000000000, 1.000000000000000000, 1.000000000000000000, 1.000000000000000000, 1.000000000000000000, 1.000000000000000000, 1.000000000000000000, 1.000000000000000000, 1.000000000000000000, 1.000000000000000000, 1.000000000000000000, 1.000000000000000000, 1.000000000000000000, 1.000000000000000000, 1.000000000000000000, 1.000000000000000000, 1.000000000000000000, 1.000000000000000000),
 ( 0.3333333333333333703, 0.3333333333333333703, 0.3333333333333333703, 0.3333333333333333703, 0.3333333333333333703, 0.3333333333333333703, 0.3333333333333333703, 0.3333333333333333703, 0.3333333333333333703, 0.3333333333333333703, 0.3333333333333333703, 0.3333333333333333703, 0.3333333333333333703, 0.3333333333333333703, 0.3333333333333333703, 0.3333333333333333703, 0.3333333333333333703, 0.3333333333333333703, 0.3333333333333333703, 0.3333333333333333703, 0.3333333333333333703, 0.3333333333333333703, 0.3333333333333333703, 0.3333333333333333703, 0.3333333333333333703, 0.3333333333333333703, 0.3333333333333333703, 0.3333333333333333703, 0.3333333333333333703, 0.3333333333333333703, 0.3333333333333333703, 0.3333333333333333703, 0.3333333333333333703, 0.3333333333333333703, 0.3333333333333333703, 0.3333333333333333703, 0.3333333333333333703, 0.3333333333333333703, 0.3333333333333333703, 0.3333333333333333703, 0.3333333333333333703, 0.3333333333333333703, 0.3333333333333333703, 0.3333333333333333703, 0.3333333333333333703, 0.3333333333333333703, 0.3333333333333333703, 0.3333333333333333703, 0.3333333333333333703, 0.3333333333333333703, 0.3333333333333333703, 0.3333333333333333703, 0.3333333333333333703, 0.3333333333333333703, 0.3333333333333333703, 0.3333333333333333703, 0.3333333333333333703, 0.3333333333333333703, 0.3333333333333333703, 0.3333333333333333703, 0.3333333333333333703, 0.3333333333333333703, 0.3333333333333333703, 0.3333333333333333703, 0.3333333333333333703, 0.3333333333333333703, 0.3333333333333333703, 0.3333333333333333703, 0.3333333333333333703, 0.3333333333333333703, 0.3333333333333333703, 0.3333333333333333703, 0.3333333333333333703, 0.3333333333333333703, 0.3333333333333333703, 0.3333333333333333703, 0.3333333333333333703, 0.3333333333333333703, 0.3333333333333333703, 0.3333333333333333703, 0.3333333333333333703, 0.3333333333333333703, 0.3333333333333333703, 0.3333333333333333703, 0.3333333333333333703, 0.3333333333333333703, 0.3333333333333333703, 0.3333333333333333703, 0.3333333333333333703, 0.3333333333333333703, 0.3333333333333333703, 0.3333333333333333703, 0.3333333333333333703, 0.3333333333333333703, 0.3333333333333333703, 0.3333333333333333703, 0.3333333333333333703, 0.3333333333333333703, 0.3333333333333333703, 0.3333333333333333703, 0.3333333333333333703, 0.3333333333333333703, 0.3333333333333333703, 0.3333333333333333703, 0.3333333333333333703, 0.3333333333333333703, 0.3333333333333333703, 0.3333333333333333703, 0.3333333333333333703, 0.3333333333333333703, 0.3333333333333333703, 0.3333333333333333703, 0.3333333333333333703, 0.3333333333333333703, 0.3333333333333333703, 0.3333333333333333703, 0.3333333333333333703, 0.3333333333333333703, 0.3333333333333333703, 0.3333333333333333703, 0.3333333333333333703, 0.3333333333333333703, 0.3333333333333333703, 0.3333333333333333703, 0.3333333333333333703, 0.3333333333333333703, 0.3333333333333333703, 0.3333333333333333703, 0.3333333333333333703, 0.3333333333333333703, 0.3333333333333333703, 0.3333333333333333703, 0.3333333333333333703, 0.3333333333333333703, 0.3333333333333333703, 0.3333333333333333703, 0.3333333333333333703, 0.3333333333333333703, 0.3333333333333333703, 0.3333333333333333703, 0.3333333333333333703, 0.3333333333333333703, 0.3333333333333333703, 0.3333333333333333703, 0.3333333333333333703, 0.3333333333333333703, 0.3333333333333333703, 0.3333333333333333703, 0.3333333333333333703, 0.3333333333333333703, 0.3333333333333333703, 0.3333333333333333703, 0.3333333333333333703, 0.3333333333333333703, 0.3333333333333333703, 0.3333333333333333703, 0.3333333333333333703, 0.3333333333333333703, 0.3333333333333333703, 0.3333333333333333703, 0.3333333333333333703, 0.3333333333333333703, 0.3333333333333333703, 0.3333333333333333703, 0.3333333333333333703, 0.3333333333333333703, 0.3333333333333333703, 0.3333333333333333703, 0.3333333333333333703, 0.3333333333333333703, 0.3333333333333333703, 0.3333333333333333703, 0.3333333333333333703, 0.3333333333333333703, 0.3333333333333333703, 0.3333333333333333703, 0.3333333333333333703, 0.3333333333333333703, 0.3333333333333333703, 0.3333333333333333703, 0.3333333333333333703, 0.3333333333333333703, 0.3333333333333333703, 0.3333333333333333703, 0.3333333333333333703, 0.3333333333333333703, 0.3333333333333333703, 0.3333333333333333703, 0.3333333333333333703, 0.3333333333333333703, 0.3333333333333333703, 0.3333333333333333703, 0.3333333333333333703, 0.3333333333333333703, 0.3333333333333333703, 0.3333333333333333703, 0.3333333333333333703, 0.3333333333333333703, 0.3333333333333333703, 0.3333333333333333703, 0.3333333333333333703, 0.3333333333333333703, 0.3333333333333333703, 0.3333333333333333703, 0.3333333333333333703, 0.3333333333333333703, 0.3333333333333333703, 0.3333333333333333703, 0.3333333333333333703, 0.3333333333333333703, 0.3333333333333333703, 0.3333333333333333703, 0.3333333333333333703, 0.3333333333333333703, 0.3333333333333333703, 0.3333333333333333703, 0.3333333333333333703, 0.3333333333333333703, 0.3333333333333333703, 0.3333333333333333703, 0.3333333333333333703, 0.3333333333333333703, 0.3333333333333333703, 0.3333333333333333703, 0.3333333333333333703, 0.3333333333333333703, 0.3333333333333333703, 0.3333333333333333703, 0.3333333333333333703, 0.3333333333333333703, 0.3333333333333333703, 0.3333333333333333703, 0.3333333333333333703, 0.3333333333333333703, 0.3333333333333333703, 0.3333333333333333703, 0.3333333333333333703, 0.3333333333333333703, 0.3333333333333333703, 0.3333333333333333703, 0.3333333333333333703, 0.3333333333333333703, 0.3333333333333333703, 0.3333333333333333703, 0.3333333333333333703, 0.3333333333333333703, 0.3333333333333333703, 0.3333333333333333703, 0.3333333333333333703, 0.3333333333333333703, 0.3333333333333333703, 0.3333333333333333703, 0.3333333333333333703, 0.3333333333333333703, 0.3333333333333333703, 0.3333333333333333703, 0.3333333333333333703, 0.3333333333333333703, 0.3333333333333333703, 0.3333333333333333703, 0.3333333333333333703, 0.3333333333333333703, 0.3333333333333333703, 0.3333333333333333703, 0.3333333333333333703, 0.3333333333333333703, 0.3333333333333333703, 0.3333333333333333703, 0.3333333333333333703, 0.3333333333333333703, 0.3333333333333333703, 0.3333333333333333703, 0.3333333333333333703, 0.3333333333333333703, 0.3333333333333333703, 0.3333333333333333703, 0.3333333333333333703, 0.3333333333333333703, 0.3333333333333333703, 0.3333333333333333703, 0.3333333333333333703, 0.3333333333333333703, 0.3333333333333333703, 0.3333333333333333703, 0.3333333333333333703, 0.3333333333333333703, 0.3333333333333333703, 0.3333333333333333703, 0.3333333333333333703, 0.3333333333333333703, 0.3333333333333333703, 0.3333333333333333703, 0.3333333333333333703, 0.3333333333333333703, 0.3333333333333333703, 0.3333333333333333703, 0.3333333333333333703, 0.3333333333333333703, 0.3333333333333333703, 0.3333333333333333703, 0.3333333333333333703, 0.3333333333333333703, 0.3333333333333333703, 0.3333333333333333703, 0.3333333333333333703, 0.3333333333333333703, 0.3333333333333333703, 0.3333333333333333703, 0.3333333333333333703, 0.3333333333333333703, 0.3333333333333333703, 0.3333333333333333703, 0.3333333333333333703, 0.3333333333333333703, 0.3333333333333333703, 0.3333333333333333703, 0.3333333333333333703, 0.3333333333333333703, 0.3333333333333333703, 0.3333333333333333703, 0.3333333333333333703, 0.3333333333333333703, 0.3333333333333333703, 0.3333333333333333703, 0.3333333333333333703, 0.3333333333333333703, 0.3333333333333333703, 0.3333333333333333703, 0.3333333333333333703, 0.3333333333333333703, 0.3333333333333333703, 0.3333333333333333703, 0.3333333333333333703, 0.3333333333333333703, 0.3333333333333333703, 0.3333333333333333703, 0.3333333333333333703, 0.3333333333333333703, 0.3333333333333333703, 0.3333333333333333703),
 ( 0.3333333333333333703, 0.3333333333333333703, 0.3333333333333333703, 0.3333333333333333703, 0.3333333333333333703, 0.3333333333333333703, 0.3333333333333333703, 0.3333333333333333703, 0.3333333333333333703, 0.3333333333333333703, 0.3333333333333333703, 0.3333333333333333703, 0.3333333333333333703, 0.3333333333333333703, 0.3333333333333333703, 0.3333333333333333703, 0.3333333333333333703, 0.3333333333333333703, 0.3333333333333333703, 0.3333333333333333703, 0.3333333333333333703, 0.3333333333333333703, 0.3333333333333333703, 0.3333333333333333703, 0.3333333333333333703, 0.3333333333333333703, 0.3333333333333333703, 0.3333333333333333703, 0.3333333333333333703, 0.3333333333333333703, 0.3333333333333333703, 0.3333333333333333703, 0.3333333333333333703, 0.3333333333333333703, 0.3333333333333333703, 0.3333333333333333703, 0.3333333333333333703, 0.3333333333333333703, 0.3333333333333333703, 0.3333333333333333703, 0.3333333333333333703, 0.3333333333333333703, 0.3333333333333333703, 0.3333333333333333703, 0.3333333333333333703, 0.3333333333333333703, 0.3333333333333333703, 0.3333333333333333703, 0.3333333333333333703, 0.3333333333333333703, 0.3333333333333333703, 0.3333333333333333703, 0.3333333333333333703, 0.3333333333333333703, 0.3333333333333333703, 0.3333333333333333703, 0.3333333333333333703, 0.3333333333333333703, 0.3333333333333333703, 0.3333333333333333703, 0.3333333333333333703, 0.3333333333333333703, 0.3333333333333333703, 0.3333333333333333703, 0.3333333333333333703, 0.3333333333333333703, 0.3333333333333333703, 0.3333333333333333703, 0.3333333333333333703, 0.3333333333333333703, 0.3333333333333333703, 0.3333333333333333703, 0.3333333333333333703, 0.3333333333333333703, 0.3333333333333333703, 0.3333333333333333703, 0.3333333333333333703, 0.3333333333333333703, 0.3333333333333333703, 0.3333333333333333703, 0.3333333333333333703, 0.3333333333333333703, 0.3333333333333333703, 0.3333333333333333703, 0.3333333333333333703, 0.3333333333333333703, 0.3333333333333333703, 0.3333333333333333703, 0.3333333333333333703, 0.3333333333333333703, 0.3333333333333333703, 0.3333333333333333703, 0.3333333333333333703, 0.3333333333333333703, 0.3333333333333333703, 0.3333333333333333703, 0.3333333333333333703, 0.3333333333333333703, 0.3333333333333333703, 0.3333333333333333703, 0.3333333333333333703, 0.3333333333333333703, 0.3333333333333333703, 0.3333333333333333703, 0.3333333333333333703, 0.3333333333333333703, 0.3333333333333333703, 0.3333333333333333703, 0.3333333333333333703, 0.3333333333333333703, 0.3333333333333333703, 0.3333333333333333703, 0.3333333333333333703, 0.3333333333333333703, 0.3333333333333333703, 0.3333333333333333703, 0.3333333333333333703, 0.3333333333333333703, 0.3333333333333333703, 0.3333333333333333703, 0.3333333333333333703, 0.3333333333333333703, 0.3333333333333333703, 0.3333333333333333703, 0.3333333333333333703, 0.3333333333333333703, 0.3333333333333333703, 0.3333333333333333703, 0.3333333333333333703, 0.3333333333333333703, 0.3333333333333333703, 0.3333333333333333703, 0.3333333333333333703, 0.3333333333333333703, 0.3333333333333333703, 0.3333333333333333703, 0.3333333333333333703, 0.3333333333333333703, 0.3333333333333333703, 0.3333333333333333703, 0.3333333333333333703, 0.3333333333333333703, 0.3333333333333333703, 0.3333333333333333703, 0.3333333333333333703, 0.3333333333333333703, 0.3333333333333333703, 0.3333333333333333703, 0.3333333333333333703, 0.3333333333333333703, 0.3333333333333333703, 0.3333333333333333703, 0.3333333333333333703, 0.3333333333333333703, 0.3333333333333333703, 0.3333333333333333703, 0.3333333333333333703, 0.3333333333333333703, 0.3333333333333333703, 0.3333333333333333703, 0.3333333333333333703, 0.3333333333333333703, 0.3333333333333333703, 0.3333333333333333703, 0.3333333333333333703, 0.3333333333333333703, 0.3333333333333333703, 0.3333333333333333703, 0.3333333333333333703, 0.3333333333333333703, 0.3333333333333333703, 0.3333333333333333703, 0.3333333333333333703, 0.3333333333333333703, 0.3333333333333333703, 0.3333333333333333703, 0.3333333333333333703, 0.3333333333333333703, 0.3333333333333333703, 0.3333333333333333703, 0.3333333333333333703, 0.3333333333333333703, 0.3333333333333333703, 0.3333333333333333703, 0.3333333333333333703, 0.3333333333333333703, 0.3333333333333333703, 0.3333333333333333703, 0.3333333333333333703, 0.3333333333333333703, 0.3333333333333333703, 0.3333333333333333703, 0.3333333333333333703, 0.3333333333333333703, 0.3333333333333333703, 0.3333333333333333703, 0.3333333333333333703, 0.3333333333333333703, 0.3333333333333333703, 0.3333333333333333703, 0.3333333333333333703, 0.3333333333333333703, 0.3333333333333333703, 0.3333333333333333703, 0.3333333333333333703, 0.3333333333333333703, 0.3333333333333333703, 0.3333333333333333703, 0.3333333333333333703, 0.3333333333333333703, 0.3333333333333333703, 0.3333333333333333703, 0.3333333333333333703, 0.3333333333333333703, 0.3333333333333333703, 0.3333333333333333703, 0.3333333333333333703, 0.3333333333333333703, 0.3333333333333333703, 0.3333333333333333703, 0.3333333333333333703, 0.3333333333333333703, 0.3333333333333333703, 0.3333333333333333703, 0.3333333333333333703, 0.3333333333333333703, 0.3333333333333333703, 0.3333333333333333703, 0.3333333333333333703, 0.3333333333333333703, 0.3333333333333333703, 0.3333333333333333703, 0.3333333333333333703, 0.3333333333333333703, 0.3333333333333333703, 0.3333333333333333703, 0.3333333333333333703, 0.3333333333333333703, 0.3333333333333333703, 0.3333333333333333703, 0.3333333333333333703, 0.3333333333333333703, 0.3333333333333333703, 0.3333333333333333703, 0.3333333333333333703, 0.3333333333333333703, 0.3333333333333333703, 0.3333333333333333703, 0.3333333333333333703, 0.3333333333333333703, 0.3333333333333333703, 0.3333333333333333703, 0.3333333333333333703, 0.3333333333333333703, 0.3333333333333333703, 0.3333333333333333703, 0.3333333333333333703, 0.3333333333333333703, 0.3333333333333333703, 0.3333333333333333703, 0.3333333333333333703, 0.3333333333333333703, 0.3333333333333333703, 0.3333333333333333703, 0.3333333333333333703, 0.3333333333333333703, 0.3333333333333333703, 0.3333333333333333703, 0.3333333333333333703, 0.3333333333333333703, 0.3333333333333333703, 0.3333333333333333703, 0.3333333333333333703, 0.3333333333333333703, 0.3333333333333333703, 0.3333333333333333703, 0.3333333333333333703, 0.3333333333333333703, 0.3333333333333333703, 0.3333333333333333703, 0.3333333333333333703, 0.3333333333333333703, 0.3333333333333333703, 0.3333333333333333703, 0.3333333333333333703, 0.3333333333333333703, 0.3333333333333333703, 0.3333333333333333703, 0.3333333333333333703, 0.3333333333333333703, 0.3333333333333333703, 0.3333333333333333703, 0.3333333333333333703, 0.3333333333333333703, 0.3333333333333333703, 0.3333333333333333703, 0.3333333333333333703, 0.3333333333333333703, 0.3333333333333333703, 0.3333333333333333703, 0.3333333333333333703, 0.3333333333333333703, 0.3333333333333333703, 0.3333333333333333703, 0.3333333333333333703, 0.3333333333333333703, 0.3333333333333333703, 0.3333333333333333703, 0.3333333333333333703, 0.3333333333333333703, 0.3333333333333333703, 0.3333333333333333703, 0.3333333333333333703, 0.3333333333333333703, 0.3333333333333333703, 0.3333333333333333703, 0.3333333333333333703, 0.3333333333333333703, 0.3333333333333333703, 0.3333333333333333703, 0.3333333333333333703, 0.3333333333333333703, 0.3333333333333333703, 0.3333333333333333703, 0.3333333333333333703, 0.3333333333333333703, 0.3333333333333333703, 0.3333333333333333703, 0.3333333333333333703, 0.3333333333333333703, 0.3333333333333333703, 0.3333333333333333703, 0.3333333333333333703, 0.3333333333333333703, 0.3333333333333333703, 0.3333333333333333703, 0.3333333333333333703, 0.3333333333333333703, 0.3333333333333333703, 0.3333333333333333703),
 ( 1.000000000000000000, 1.000000000000000000, 1.000000000000000000, 1.000000000000000000, 1.000000000000000000, 1.000000000000000000, 1.000000000000000000, 1.000000000000000000, 1.000000000000000000, 1.000000000000000000, 1.000000000000000000, 1.000000000000000000, 1.000000000000000000, 1.000000000000000000, 1.000000000000000000, 1.000000000000000000, 1.000000000000000000, 1.000000000000000000, 1.000000000000000000, 1.000000000000000000, 1.000000000000000000, 1.000000000000000000, 1.000000000000000000, 1.000000000000000000, 1.000000000000000000, 1.000000000000000000, 1.000000000000000000, 1.000000000000000000, 1.000000000000000000, 1.000000000000000000, 1.000000000000000000, 1.000000000000000000, 1.000000000000000000, 1.000000000000000000, 1.000000000000000000, 1.000000000000000000, 1.000000000000000000, 1.000000000000000000, 1.000000000000000000, 1.000000000000000000, 1.000000000000000000, 1.000000000000000000, 1.000000000000000000, 1.000000000000000000, 1.000000000000000000, 1.000000000000000000, 1.000000000000000000, 1.000000000000000000, 1.000000000000000000, 1.000000000000000000, 1.000000000000000000, 1.000000000000000000, 1.000000000000000000, 1.000000000000000000, 1.000000000000000000, 1.000000000000000000, 1.000000000000000000, 1.000000000000000000, 1.000000000000000000, 1.000000000000000000, 1.000000000000000000, 1.000000000000000000, 1.000000000000000000, 1.000000000000000000, 1.000000000000000000, 1.000000000000000000, 1.000000000000000000, 1.000000000000000000, 1.000000000000000000, 1.000000000000000000, 1.000000000000000000, 1.000000000000000000, 1.000000000000000000, 1.000000000000000000, 1.000000000000000000, 1.000000000000000000, 1.000000000000000000, 1.000000000000000000, 1.000000000000000000, 1.000000000000000000, 1.000000000000000000, 1.000000000000000000, 1.000000000000000000, 1.000000000000000000, 1.000000000000000000, 1.000000000000000000, 1.000000000000000000, 1.000000000000000000, 1.000000000000000000, 1.000000000000000000, 1.000000000000000000, 1.000000000000000000, 1.000000000000000000, 1.000000000000000000, 1.000000000000000000, 1.000000000000000000, 1.000000000000000000, 1.000000000000000000, 1.000000000000000000, 1.000000000000000000, 1.000000000000000000, 1.000000000000000000, 1.000000000000000000, 1.000000000000000000, 1.000000000000000000, 1.000000000000000000, 1.000000000000000000, 1.000000000000000000, 1.000000000000000000, 1.000000000000000000, 1.000000000000000000, 1.000000000000000000, 1.000000000000000000, 1.000000000000000000, 1.000000000000000000, 1.000000000000000000, 1.000000000000000000, 1.000000000000000000, 1.000000000000000000, 1.000000000000000000, 1.000000000000000000, 1.000000000000000000, 1.000000000000000000, 1.000000000000000000, 1.000000000000000000, 1.000000000000000000, 1.000000000000000000, 1.000000000000000000, 1.000000000000000000, 1.000000000000000000, 1.000000000000000000, 1.000000000000000000, 1.000000000000000000, 1.000000000000000000, 1.000000000000000000, 1.000000000000000000, 1.000000000000000000, 1.000000000000000000, 1.000000000000000000, 1.000000000000000000, 1.000000000000000000, 1.000000000000000000, 1.000000000000000000, 1.000000000000000000, 1.000000000000000000, 1.000000000000000000, 1.000000000000000000, 1.000000000000000000, 1.000000000000000000, 1.000000000000000000, 1.000000000000000000, 1.000000000000000000, 1.000000000000000000, 1.000000000000000000, 1.000000000000000000, 1.000000000000000000, 1.000000000000000000, 1.000000000000000000, 1.000000000000000000, 1.000000000000000000, 1.000000000000000000, 1.000000000000000000, 1.000000000000000000, 1.000000000000000000, 1.000000000000000000, 1.000000000000000000, 1.000000000000000000, 1.000000000000000000, 1.000000000000000000, 1.000000000000000000, 1.000000000000000000, 1.000000000000000000, 1.000000000000000000, 1.000000000000000000, 1.000000000000000000, 1.000000000000000000, 1.000000000000000000, 1.000000000000000000, 1.000000000000000000, 1.000000000000000000, 1.000000000000000000, 1.000000000000000000, 1.000000000000000000, 1.000000000000000000, 1.000000000000000000, 1.000000000000000000, 1.000000000000000000, 1.000000000000000000, 1.000000000000000000, 1.000000000000000000, 1.000000000000000000, 1.000000000000000000, 1.000000000000000000, 1.000000000000000000, 1.000000000000000000, 1.000000000000000000, 1.000000000000000000, 1.000000000000000000, 1.000000000000000000, 1.000000000000000000, 1.000000000000000000, 1.000000000000000000, 1.000000000000000000, 1.000000000000000000, 1.000000000000000000, 1.000000000000000000, 1.000000000000000000, 1.000000000000000000, 1.000000000000000000, 1.000000000000000000, 1.000000000000000000, 1.000000000000000000, 1.000000000000000000, 1.000000000000000000, 1.000000000000000000, 1.000000000000000000, 1.000000000000000000, 1.000000000000000000, 1.000000000000000000, 1.000000000000000000, 1.000000000000000000, 1.000000000000000000, 1.000000000000000000, 1.000000000000000000, 1.000000000000000000, 1.000000000000000000, 1.000000000000000000, 1.000000000000000000, 1.000000000000000000, 1.000000000000000000, 1.000000000000000000, 1.000000000000000000, 1.000000000000000000, 1.000000000000000000, 1.000000000000000000, 1.000000000000000000, 1.000000000000000000, 1.000000000000000000, 1.000000000000000000, 1.000000000000000000, 1.000000000000000000, 1.000000000000000000, 1.000000000000000000, 1.000000000000000000, 1.000000000000000000, 1.000000000000000000, 1.000000000000000000, 1.000000000000000000, 1.000000000000000000, 1.000000000000000000, 1.000000000000000000, 1.000000000000000000, 1.000000000000000000, 1.000000000000000000, 1.000000000000000000, 1.000000000000000000, 1.000000000000000000, 1.000000000000000000, 1.000000000000000000, 1.000000000000000000, 1.000000000000000000, 1.000000000000000000, 1.000000000000000000, 1.000000000000000000, 1.000000000000000000, 1.000000000000000000, 1.000000000000000000, 1.000000000000000000, 1.000000000000000000, 1.000000000000000000, 1.000000000000000000, 1.000000000000000000, 1.000000000000000000, 1.000000000000000000, 1.000000000000000000, 1.000000000000000000, 1.000000000000000000, 1.000000000000000000, 1.000000000000000000, 1.000000000000000000, 1.000000000000000000, 1.000000000000000000, 1.000000000000000000, 1.000000000000000000, 1.000000000000000000, 1.000000000000000000, 1.000000000000000000, 1.000000000000000000, 1.000000000000000000, 1.000000000000000000, 1.000000000000000000, 1.000000000000000000, 1.000000000000000000, 1.000000000000000000, 1.000000000000000000, 1.000000000000000000, 1.000000000000000000, 1.000000000000000000, 1.000000000000000000, 1.000000000000000000, 1.000000000000000000, 1.000000000000000000, 1.000000000000000000, 1.000000000000000000, 1.000000000000000000, 1.000000000000000000, 1.000000000000000000, 1.000000000000000000, 1.000000000000000000, 1.000000000000000000, 1.000000000000000000, 1.000000000000000000, 1.000000000000000000, 1.000000000000000000, 1.000000000000000000, 1.000000000000000000, 1.000000000000000000, 1.000000000000000000, 1.000000000000000000, 1.000000000000000000, 1.000000000000000000, 1.000000000000000000, 1.000000000000000000, 1.000000000000000000, 1.000000000000000000, 1.000000000000000000, 1.000000000000000000, 1.000000000000000000, 1.000000000000000000, 1.000000000000000000, 1.000000000000000000, 1.000000000000000000, 1.000000000000000000, 1.000000000000000000, 1.000000000000000000, 1.000000000000000000, 1.000000000000000000, 1.000000000000000000, 1.000000000000000000, 1.000000000000000000) ) ) 
 REPRESENTATION_ITEM ( '' )  SURFACE ( )  );
#14511 = CIRCLE ( 'NONE', #8043, 5.000000000000000888 ) ;
#14512 = EDGE_CURVE ( 'NONE', #645, #9941, #10948, .T. ) ;
#14513 = CARTESIAN_POINT ( 'NONE',  ( -18.93763370444446181, -0.7340653299870684156, -219.7345063954518594 ) ) ;
#14514 = CARTESIAN_POINT ( 'NONE',  ( 12.46318849118074112, 25.01309605388695445, -216.9820503660967859 ) ) ;
#14515 = CARTESIAN_POINT ( 'NONE',  ( 24.57222455393806015, 12.08236629421828212, -229.7319216558644541 ) ) ;
#14516 = CARTESIAN_POINT ( 'NONE',  ( 0.000000000000000000, 0.000000000000000000, -60.00000000000001421 ) ) ;
#14517 = CARTESIAN_POINT ( 'NONE',  ( -11.51027863121307782, -1.790843358437596677, -225.0773512427349203 ) ) ;
#14518 = CARTESIAN_POINT ( 'NONE',  ( -11.06377138986482933, -15.30386857868810857, -217.0411070525910873 ) ) ;
#14519 = CARTESIAN_POINT ( 'NONE',  ( 9.358654279681809740, -11.94480763145079472, -229.8864256833185777 ) ) ;
#14520 = DIRECTION ( 'NONE',  ( 0.000000000000000000, 0.000000000000000000, 1.000000000000000000 ) ) ;
#14521 = DIRECTION ( 'NONE',  ( 0.000000000000000000, 0.000000000000000000, -1.000000000000000000 ) ) ;
#14522 = CARTESIAN_POINT ( 'NONE',  ( -1.696080206444520844, 14.74162257415073540, -222.2455536759108838 ) ) ;
#14523 = CARTESIAN_POINT ( 'NONE',  ( 13.42370487565828796, -6.089723759188163221, -217.7532606872487406 ) ) ;
#14524 = CARTESIAN_POINT ( 'NONE',  ( 15.50779141722566656, -5.694711448414747856, -219.6385356284298211 ) ) ;
#14525 = CIRCLE ( 'NONE', #16631, 23.00000000000000000 ) ;
#14526 = CARTESIAN_POINT ( 'NONE',  ( -16.28025842329327944, 6.985656672962045732, -231.4191468057695715 ) ) ;
#14527 = CARTESIAN_POINT ( 'NONE',  ( 22.20554449732931346, 18.01468431515759860, -218.9348803756412849 ) ) ;
#14528 = CARTESIAN_POINT ( 'NONE',  ( 11.00580183749007190, 25.74996642444834904, -225.8602305833924788 ) ) ;
#14529 = ORIENTED_EDGE ( 'NONE', *, *, #14233, .T. ) ;
#14530 = CARTESIAN_POINT ( 'NONE',  ( 7.898002370961310525, -21.57266348603731387, -216.1546105971396798 ) ) ;
#14531 = FACE_BOUND ( 'NONE', #13200, .T. ) ;
#14532 = CARTESIAN_POINT ( 'NONE',  ( 4.966801760238292118, 27.41406605988239420, -216.4490579899774900 ) ) ;
#14533 = CARTESIAN_POINT ( 'NONE',  ( -8.929606928624414408, 11.65278034267609186, -219.1999234847403386 ) ) ;
#14534 = CARTESIAN_POINT ( 'NONE',  ( -19.29805292978571885, -8.785194383212417080, -233.3520286081516133 ) ) ;
#14535 = CARTESIAN_POINT ( 'NONE',  ( -16.65698539163286540, 11.03290537638306112, -233.6474915129378758 ) ) ;
#14536 = FACE_OUTER_BOUND ( 'NONE', #4522, .T. ) ;
#14537 = CARTESIAN_POINT ( 'NONE',  ( 0.000000000000000000, 0.000000000000000000, 77.51594804401857175 ) ) ;
#14538 = CARTESIAN_POINT ( 'NONE',  ( -7.266348978356541366, 16.38312187400933340, -217.9429203627011873 ) ) ;
#14539 = CARTESIAN_POINT ( 'NONE',  ( -21.28804099221702018, -0.9277163183344186992, -219.0000000002572733 ) ) ;
#14540 = CARTESIAN_POINT ( 'NONE',  ( -14.00380962569832199, 8.747390586476997854, -231.7950903513155936 ) ) ;
#14541 = VECTOR ( 'NONE', #2426, 1000.000000000000000 ) ;
#14542 = CARTESIAN_POINT ( 'NONE',  ( 21.39553407250273054, 8.453402029343234148, -217.9531594780983141 ) ) ;
#14543 = DIRECTION ( 'NONE',  ( 1.000000000000000000, 0.000000000000000000, 0.000000000000000000 ) ) ;
#14544 = ORIENTED_EDGE ( 'NONE', *, *, #22017, .F. ) ;
#14545 = CARTESIAN_POINT ( 'NONE',  ( -1.268862717067444024, 15.25222216985846480, -229.0661283592426116 ) ) ;
#14546 = CARTESIAN_POINT ( 'NONE',  ( -20.76924187596804217, -21.50248317380421170, -228.3679492147379335 ) ) ;
#14547 = CARTESIAN_POINT ( 'NONE',  ( 18.50911814746675788, 15.92944434255054453, -232.0449215596906072 ) ) ;
#14548 = CARTESIAN_POINT ( 'NONE',  ( -9.869267615102224056, -25.54258770546914903, -218.7733540664615930 ) ) ;
#14549 = DIRECTION ( 'NONE',  ( -1.000000000000000000, 1.224646799147353454E-16, 0.000000000000000000 ) ) ;
#14550 = CARTESIAN_POINT ( 'NONE',  ( -25.64868633208605786, 12.30364128039660798, -229.0020209687957049 ) ) ;
#14551 = CARTESIAN_POINT ( 'NONE',  ( 18.24334571313621467, -21.83696521683136282, -220.5798317591433886 ) ) ;
#14552 = CARTESIAN_POINT ( 'NONE',  ( 8.179023008129211902, 20.84698146175953681, -218.6376653143925921 ) ) ;
#14553 = CARTESIAN_POINT ( 'NONE',  ( -13.37045227479810094, 5.250293981428504786, -224.2914120185227205 ) ) ;
#14554 = CARTESIAN_POINT ( 'NONE',  ( -9.503027668167838726, 6.959046566381404730, -225.7241663910276941 ) ) ;
#14555 = CARTESIAN_POINT ( 'NONE',  ( -10.33268794075157082, -17.24452578398873115, -232.5240627438851959 ) ) ;
#14556 = CARTESIAN_POINT ( 'NONE',  ( 15.06072304412464291, 3.291435955319735651, -218.8606307204261725 ) ) ;
#14557 = VECTOR ( 'NONE', #10845, 1000.000000000000000 ) ;
#14558 = CYLINDRICAL_SURFACE ( 'NONE', #5493, 20.99999999999999645 ) ;
#14559 = CARTESIAN_POINT ( 'NONE',  ( -18.91688971021567767, -12.73417920357403688, -235.2301191595167040 ) ) ;
#14560 = CARTESIAN_POINT ( 'NONE',  ( 1.656472371294090085, 27.29382523973669095, -230.4991099578876117 ) ) ;
#14561 = ADVANCED_FACE ( 'NONE', ( #711 ), #16139, .T. ) ;
#14562 = CARTESIAN_POINT ( 'NONE',  ( 15.39025625686376841, 1.044190007782545226, -218.9203249718910911 ) ) ;
#14563 = CARTESIAN_POINT ( 'NONE',  ( -11.55316006017064012, 19.79513644261079719, -232.3088878043970453 ) ) ;
#14564 = CARTESIAN_POINT ( 'NONE',  ( 17.04685026979186446, 18.05617612716381970, -216.0910122987878310 ) ) ;
#14565 = VERTEX_POINT ( 'NONE', #21287 ) ;
#14566 = CARTESIAN_POINT ( 'NONE',  ( 5.446054363465077763, -20.62119468428589997, -218.5301445808800622 ) ) ;
#14567 = CARTESIAN_POINT ( 'NONE',  ( -5.805911442544755552, -26.83424102279996504, -229.6222293353685302 ) ) ;
#14568 = CARTESIAN_POINT ( 'NONE',  ( 27.75679124201660741, 4.911524026080384075, -221.4430403652340829 ) ) ;
#14569 = CARTESIAN_POINT ( 'NONE',  ( 19.06435866915521515, -20.24829071055443563, -218.8318535520223804 ) ) ;
#14570 = CARTESIAN_POINT ( 'NONE',  ( -15.46216926290318305, -2.495270579625169738, -221.2150947962298631 ) ) ;
#14571 = CIRCLE ( 'NONE', #5210, 17.50000000000007816 ) ;
#14572 = CARTESIAN_POINT ( 'NONE',  ( -9.294226473174397540, -12.00440878504259601, -219.6990993854437875 ) ) ;
#14573 = CARTESIAN_POINT ( 'NONE',  ( 7.067550969709256670, 17.75197616922148569, -219.3387126207321955 ) ) ;
#14574 = DIRECTION ( 'NONE',  ( 1.000000000000000000, 0.000000000000000000, 0.000000000000000000 ) ) ;
#14575 = CARTESIAN_POINT ( 'NONE',  ( 14.18323607655884722, 3.286047475533308226, -222.8710065128477140 ) ) ;
#14576 = CARTESIAN_POINT ( 'NONE',  ( 5.017623471397871349, 29.83561274492976878, -222.9769172135417250 ) ) ;
#14577 = CARTESIAN_POINT ( 'NONE',  ( -0.7879796667336372851, 21.22375955577181372, -219.1554080315090118 ) ) ;
#14578 = CARTESIAN_POINT ( 'NONE',  ( 20.72180063689699026, -9.651256082433341987, -234.7026181832539180 ) ) ;
#14579 = ORIENTED_EDGE ( 'NONE', *, *, #10780, .T. ) ;
#14580 = CARTESIAN_POINT ( 'NONE',  ( 15.88043104796248528, 11.88135572392608807, -216.2525917828042168 ) ) ;
#14581 = EDGE_CURVE ( 'NONE', #4133, #12432, #9874, .T. ) ;
#14582 = CARTESIAN_POINT ( 'NONE',  ( -22.38528940623734798, 16.50235888036280230, -227.1443357386333162 ) ) ;
#14583 = CARTESIAN_POINT ( 'NONE',  ( -17.91769793922991028, 3.277678596821882007, -219.5526088240203819 ) ) ;
#14584 = CARTESIAN_POINT ( 'NONE',  ( -5.980659577089002532, -19.45286470896024156, -217.9322865582606710 ) ) ;
#14585 = CYLINDRICAL_SURFACE ( 'NONE', #1133, 17.50000000000000355 ) ;
#14586 = FACE_OUTER_BOUND ( 'NONE', #6005, .T. ) ;
#14587 = CARTESIAN_POINT ( 'NONE',  ( 4.559463107227270662, 13.27337529356814017, -226.9596205199204633 ) ) ;
#14588 = CARTESIAN_POINT ( 'NONE',  ( 16.32467020957917114, -16.75837631771952019, -218.4891864258081853 ) ) ;
#14589 = ADVANCED_FACE ( 'NONE', ( #2913 ), #7482, .T. ) ;
#14590 = CARTESIAN_POINT ( 'NONE',  ( -20.00523085820573499, 3.356386534894876927, -232.9491364426554298 ) ) ;
#14591 = AXIS2_PLACEMENT_3D ( 'NONE', #21744, #1161, #13313 ) ;
#14592 = CARTESIAN_POINT ( 'NONE',  ( -7.460068573003235670, -29.58770008691625364, -228.1902472473001637 ) ) ;
#14593 = CARTESIAN_POINT ( 'NONE',  ( -3.855805549595750392, 26.68244055262801950, -232.4569730455296508 ) ) ;
#14594 = CARTESIAN_POINT ( 'NONE',  ( -4.695076324262313250, 31.85502299853856201, -223.8918597786031341 ) ) ;
#14595 = ORIENTED_EDGE ( 'NONE', *, *, #12595, .T. ) ;
#14596 = CARTESIAN_POINT ( 'NONE',  ( -22.17339560624464312, 16.26550580028390769, -232.0582861498566274 ) ) ;
#14597 = CARTESIAN_POINT ( 'NONE',  ( 18.84909589690502685, -4.856542942594316514, -217.9726137486037771 ) ) ;
#14598 = CARTESIAN_POINT ( 'NONE',  ( -23.13321191529080068, -9.483104312044424944, 3.241338891325622473 ) ) ;
#14599 = DIRECTION ( 'NONE',  ( 1.000000000000000000, 0.000000000000000000, -0.000000000000000000 ) ) ;
#14600 = CARTESIAN_POINT ( 'NONE',  ( -16.39453490553961856, 20.24836633112041184, -233.1722131570092245 ) ) ;
#14601 = CARTESIAN_POINT ( 'NONE',  ( -4.226568860449858356, -15.17239585821433678, -217.2407179915541349 ) ) ;
#14602 = CARTESIAN_POINT ( 'NONE',  ( 27.36047156164216787, -8.591464759722228450, -221.3690063136810977 ) ) ;
#14603 = CARTESIAN_POINT ( 'NONE',  ( -11.46843428684449151, 6.508406145394057596, -225.7212143570321814 ) ) ;
#14604 = CARTESIAN_POINT ( 'NONE',  ( -29.50764134580612463, 7.783340782857166573, -219.9768238800827191 ) ) ;
#14605 = CARTESIAN_POINT ( 'NONE',  ( -4.824452364631481416, 22.01523768541901305, -216.8350837474290245 ) ) ;
#14606 = CARTESIAN_POINT ( 'NONE',  ( -29.30406754532526037, 5.063969254119831120, -221.8212091093853076 ) ) ;
#14607 = CARTESIAN_POINT ( 'NONE',  ( 14.23294950300690331, 6.961167337017927892, -222.0879133937260974 ) ) ;
#14608 = CARTESIAN_POINT ( 'NONE',  ( -14.04270955969662360, -23.25437626513260980, -222.0989702864435174 ) ) ;
#14609 = CIRCLE ( 'NONE', #4879, 1.000000000000013323 ) ;
#14610 = ORIENTED_EDGE ( 'NONE', *, *, #3080, .F. ) ;
#14611 = STYLED_ITEM ( 'NONE', ( #13290 ), #20620 ) ;
#14612 = CARTESIAN_POINT ( 'NONE',  ( 6.566035546683759883, 15.06745272174450712, -218.8330720708048034 ) ) ;
#14613 = CARTESIAN_POINT ( 'NONE',  ( -11.83954511762131112, 10.58068896997146346, -226.6171226499791089 ) ) ;
#14614 = CARTESIAN_POINT ( 'NONE',  ( -14.64425879132321384, 10.88727730234500868, -217.2315376225554644 ) ) ;
#14615 = CARTESIAN_POINT ( 'NONE',  ( -28.53682043726378836, -3.412203979905605866, -221.0207037827091767 ) ) ;
#14616 = LINE ( 'NONE', #21671, #15069 ) ;
#14617 = ORIENTED_EDGE ( 'NONE', *, *, #3361, .T. ) ;
#14618 = CARTESIAN_POINT ( 'NONE',  ( -15.15110768032078070, 3.517015312212880218, -219.5479300368539270 ) ) ;
#14619 = CARTESIAN_POINT ( 'NONE',  ( -8.876630286717240637, -14.53920553942005256, -232.5681369007955368 ) ) ;
#14620 = CARTESIAN_POINT ( 'NONE',  ( 13.50203797739595402, 0.4864885784468633290, -227.9631964266715443 ) ) ;
#14621 = CARTESIAN_POINT ( 'NONE',  ( 0.4042326456706432647, 15.50845657815858303, -219.2680337625893401 ) ) ;
#14622 = PLANE ( 'NONE',  #18451 ) ;
#14623 = CIRCLE ( 'NONE', #7071, 22.56777165119825668 ) ;
#14624 = CARTESIAN_POINT ( 'NONE',  ( -19.35155980425159683, 1.157993580480985552, -230.3698774940947942 ) ) ;
#14625 = ADVANCED_FACE ( 'NONE', ( #8119 ), #16696, .T. ) ;
#14626 = CARTESIAN_POINT ( 'NONE',  ( 19.29971334243027314, 24.42889259816135095, -228.2141526116784291 ) ) ;
#14627 = CARTESIAN_POINT ( 'NONE',  ( 18.29617186523616468, 23.20920553663278341, -223.4372550713720216 ) ) ;
#14628 = DIRECTION ( 'NONE',  ( 0.000000000000000000, 0.000000000000000000, -1.000000000000000000 ) ) ;
#14629 = CARTESIAN_POINT ( 'NONE',  ( -13.08850661186922260, -6.354795836388488439, -231.9371199848366984 ) ) ;
#14630 = CARTESIAN_POINT ( 'NONE',  ( -28.46519324992292965, -8.397260794665152517, -225.6705986409035347 ) ) ;
#14631 = CARTESIAN_POINT ( 'NONE',  ( 0.000000000000000000, 0.000000000000000000, -24.99999999999999645 ) ) ;
#14632 = CARTESIAN_POINT ( 'NONE',  ( -11.24282496690421596, 12.44430180464951086, -232.4405891940542404 ) ) ;
#14633 = CARTESIAN_POINT ( 'NONE',  ( -6.079211283031130897, 16.94466709905296753, -232.9163774423793711 ) ) ;
#14634 = CARTESIAN_POINT ( 'NONE',  ( 19.51310828881794990, -1.786742129898636344, -215.1201286626718741 ) ) ;
#14635 = CARTESIAN_POINT ( 'NONE',  ( 15.05575868828727515, -2.428864548505686560, -227.9368649688638584 ) ) ;
#14636 = CARTESIAN_POINT ( 'NONE',  ( -13.81390866287826746, 1.832988708064121175, -224.4361041349432639 ) ) ;
#14637 = CARTESIAN_POINT ( 'NONE',  ( 13.82984244654956107, 22.51831320572884820, -232.1830460045772213 ) ) ;
#14638 = CARTESIAN_POINT ( 'NONE',  ( 16.01130065545721592, 20.79417322911648114, -220.9619135886794652 ) ) ;
#14639 = VERTEX_POINT ( 'NONE', #2396 ) ;
#14640 = CARTESIAN_POINT ( 'NONE',  ( 11.05135090310477786, -21.04892152267781569, -234.3520113253972568 ) ) ;
#14641 = CARTESIAN_POINT ( 'NONE',  ( 16.91879448796214191, 0.8271603773820436212, -230.0510230802265710 ) ) ;
#14642 = SHAPE_REPRESENTATION ( 'top housing_top housing', ( #6677 ), #2013 ) ;
#14643 = CARTESIAN_POINT ( 'NONE',  ( 4.754245974719506940, 31.05377813473586102, -220.6166503949300193 ) ) ;
#14644 = CARTESIAN_POINT ( 'NONE',  ( -17.15943377049709184, 17.77880916606822836, -233.2929083076029144 ) ) ;
#14645 = CARTESIAN_POINT ( 'NONE',  ( 26.05530571436537457, -9.878918321867194763, -229.2327836737675284 ) ) ;
#14646 = CARTESIAN_POINT ( 'NONE',  ( -3.082945806077231676, 30.69897765966285874, -224.2387254578930822 ) ) ;
#14647 = CARTESIAN_POINT ( 'NONE',  ( -25.00000000000001066, 0.000000000000000000, -75.00000000000000000 ) ) ;
#14648 = CARTESIAN_POINT ( 'NONE',  ( 2.000982021813747291, 12.72833461843010205, -228.3416607300594308 ) ) ;
#14649 = CARTESIAN_POINT ( 'NONE',  ( 16.53896178738450828, 2.691624496798088462, -232.5974196329879078 ) ) ;
#14650 = CARTESIAN_POINT ( 'NONE',  ( -22.99617382825321599, 17.18101613848176967, -230.9512687019100099 ) ) ;
#14651 = CARTESIAN_POINT ( 'NONE',  ( 24.57222455393806015, 12.08236629421828212, -229.7319216558644541 ) ) ;
#14652 = DIRECTION ( 'NONE',  ( 1.224646799147353207E-16, 1.000000000000000000, 0.000000000000000000 ) ) ;
#14653 = ORIENTED_EDGE ( 'NONE', *, *, #18200, .F. ) ;
#14654 = CARTESIAN_POINT ( 'NONE',  ( 0.9879969248128627202, 20.02408072508558945, -218.2055348255049410 ) ) ;
#14655 = CARTESIAN_POINT ( 'NONE',  ( -18.44715843167851688, -19.86029123650958184, -231.9563062773970046 ) ) ;
#14656 = CARTESIAN_POINT ( 'NONE',  ( 10.57926812561479757, 10.00910231482511215, -225.8341706491384286 ) ) ;
#14657 = CARTESIAN_POINT ( 'NONE',  ( -4.239735564391798661, -14.20018808486349116, -230.2489621771221380 ) ) ;
#14658 = CARTESIAN_POINT ( 'NONE',  ( 21.56733749965854940, 0.4285765077750016694, -222.0295450773661230 ) ) ;
#14659 = CARTESIAN_POINT ( 'NONE',  ( -24.18895665211001500, 11.26087434487096139, -231.0040666710689550 ) ) ;
#14660 = CARTESIAN_POINT ( 'NONE',  ( 8.158223302632384488, -13.44420475212243993, -229.3230086144918403 ) ) ;
#14661 = EDGE_CURVE ( 'NONE', #15877, #10662, #14984, .T. ) ;
#14662 = CARTESIAN_POINT ( 'NONE',  ( 6.136979247480394584, 21.37054498543370684, -230.9985475420231467 ) ) ;
#14663 = CARTESIAN_POINT ( 'NONE',  ( -26.11114532382342901, 12.73400870066318902, -227.7653936945517046 ) ) ;
#14664 = CARTESIAN_POINT ( 'NONE',  ( -31.76239872120898511, 5.177298019713663990, -226.5714959923072342 ) ) ;
#14665 = CARTESIAN_POINT ( 'NONE',  ( -14.98971194994906853, -6.742389346827670771, -223.0360336987919823 ) ) ;
#14666 = CARTESIAN_POINT ( 'NONE',  ( 12.71499452845021416, 2.172589307656224378, -223.9381607050773084 ) ) ;
#14667 = FACE_BOUND ( 'NONE', #14701, .T. ) ;
#14668 = CARTESIAN_POINT ( 'NONE',  ( -12.42228566111607968, -8.873047627549107474, -232.6540845750675999 ) ) ;
#14669 = CARTESIAN_POINT ( 'NONE',  ( 3.291078285693179950, 23.55624334554876498, -217.3208248278388623 ) ) ;
#14670 = CARTESIAN_POINT ( 'NONE',  ( 17.57135037026572277, 0.09191994211922807634, -232.8447871904542410 ) ) ;
#14671 = CARTESIAN_POINT ( 'NONE',  ( -9.222253059793434460, 13.27185325399938165, -229.0864811363590547 ) ) ;
#14672 = CARTESIAN_POINT ( 'NONE',  ( 10.61539692146153691, 8.157890242340682718, -227.5705019877536301 ) ) ;
#14673 = ORIENTED_EDGE ( 'NONE', *, *, #2939, .F. ) ;
#14674 = CARTESIAN_POINT ( 'NONE',  ( 3.849154133940814848, -15.34907234289524958, -223.0340372416051196 ) ) ;
#14675 = ORIENTED_EDGE ( 'NONE', *, *, #12898, .T. ) ;
#14676 = CARTESIAN_POINT ( 'NONE',  ( -1.432270239486107766, -17.91381153981195951, -219.1344183636291802 ) ) ;
#14677 = CARTESIAN_POINT ( 'NONE',  ( 13.49011766416699842, 7.659170998773840111, -228.1905628957712793 ) ) ;
#14678 = CARTESIAN_POINT ( 'NONE',  ( 10.24538335401965661, -11.82980241027587276, -219.3753974371782363 ) ) ;
#14679 = CARTESIAN_POINT ( 'NONE',  ( -22.05223281125446633, 0.4748437386657422543, -217.8785187290425256 ) ) ;
#14680 = CARTESIAN_POINT ( 'NONE',  ( -8.803769170443210612, -17.82266517633203406, -233.6972128408098683 ) ) ;
#14681 = CARTESIAN_POINT ( 'NONE',  ( 4.894897393135387631, 18.48819632322109996, -230.2131424875790628 ) ) ;
#14682 = CARTESIAN_POINT ( 'NONE',  ( 0.000000000000000000, 0.000000000000000000, -69.99999999999998579 ) ) ;
#14683 = CARTESIAN_POINT ( 'NONE',  ( 15.58465056415575312, 2.812367138262562349, -229.5090343034091234 ) ) ;
#14684 = CARTESIAN_POINT ( 'NONE',  ( 7.168644370073567806, 19.32044210858112265, -233.1278450877711634 ) ) ;
#14685 = CARTESIAN_POINT ( 'NONE',  ( 8.686008240521225332, 26.11221116136006515, -227.6539570933143466 ) ) ;
#14686 = CARTESIAN_POINT ( 'NONE',  ( 7.023652882903417272, -9.473209335044964874, -223.0206350579724983 ) ) ;
#14687 = CARTESIAN_POINT ( 'NONE',  ( 19.40629804599390340, 15.10110417999774057, -216.3942729496570223 ) ) ;
#14688 = CARTESIAN_POINT ( 'NONE',  ( -24.40185606299549192, 11.66496215664722236, -221.9473669705449765 ) ) ;
#14689 = CARTESIAN_POINT ( 'NONE',  ( -18.63458318964815774, 8.046101765467303935, -217.8151248213926863 ) ) ;
#14690 = CARTESIAN_POINT ( 'NONE',  ( -1.339836966046043631, -21.49735173129188581, -217.9043760890963313 ) ) ;
#14691 = LINE ( 'NONE', #19836, #9766 ) ;
#14692 = FACE_OUTER_BOUND ( 'NONE', #5114, .T. ) ;
#14693 = CARTESIAN_POINT ( 'NONE',  ( 13.49011766416699842, 7.659170998773840111, -228.1905628957712793 ) ) ;
#14694 = CARTESIAN_POINT ( 'NONE',  ( 16.49868092868510061, -6.867418253114158766, -220.9302697977882133 ) ) ;
#14695 = CARTESIAN_POINT ( 'NONE',  ( -16.27882490622757672, 1.520697279646460398, -219.2607721384596289 ) ) ;
#14696 = TOROIDAL_SURFACE ( 'NONE', #12887, 24.63401512838761320, 3.000000000000035083 ) ;
#14697 = CARTESIAN_POINT ( 'NONE',  ( -6.052919920376759855, -15.38051382379660836, -218.0337201863237624 ) ) ;
#14698 = APPLICATION_PROTOCOL_DEFINITION ( 'draft international standard', 'automotive_design', 1998, #16773 ) ;
#14699 = CARTESIAN_POINT ( 'NONE',  ( 4.301648988406530094, 13.23079486486395240, -223.2766268961034655 ) ) ;
#14700 = CARTESIAN_POINT ( 'NONE',  ( -2.577721557973523314, 25.83760098923793791, -215.4660676095525389 ) ) ;
#14701 = EDGE_LOOP ( 'NONE', ( #14149, #1476 ) ) ;
#14702 = CARTESIAN_POINT ( 'NONE',  ( -20.18153419852512442, 14.25141268122526483, -233.5059133483111964 ) ) ;
#14703 = CARTESIAN_POINT ( 'NONE',  ( -22.19673167533144564, -9.562764463827019057, -233.1557790568585062 ) ) ;
#14704 = CARTESIAN_POINT ( 'NONE',  ( -23.13924380385313739, -9.465003506282521073, -3.243783901925690216 ) ) ;
#14705 = CARTESIAN_POINT ( 'NONE',  ( -20.86724456400193617, 9.673627921070774960, -2.620012337426697258 ) ) ;
#14706 = CARTESIAN_POINT ( 'NONE',  ( -9.749377714296398878, 10.28442384816749922, -229.3722863967025205 ) ) ;
#14707 = CARTESIAN_POINT ( 'NONE',  ( -14.64285150619984677, -17.93374633926643824, -235.3168067477300838 ) ) ;
#14708 = CARTESIAN_POINT ( 'NONE',  ( 23.36729170583618398, -5.500043712341283531, -232.1593072787115375 ) ) ;
#14709 = CARTESIAN_POINT ( 'NONE',  ( -8.823862513872974489, 14.92351368520778898, -217.1499513473673346 ) ) ;
#14710 = CARTESIAN_POINT ( 'NONE',  ( 17.92683513449900445, 4.153309877386362814, -218.0960491240478234 ) ) ;
#14711 = EDGE_LOOP ( 'NONE', ( #2422, #18952, #18949, #18008, #8073, #14673 ) ) ;
#14712 = CARTESIAN_POINT ( 'NONE',  ( -6.072587425033909803, 24.65158735603439055, -217.4249768037189767 ) ) ;
#14713 = FACE_OUTER_BOUND ( 'NONE', #17763, .T. ) ;
#14714 = CARTESIAN_POINT ( 'NONE',  ( 25.53003411612920459, 7.940385729200389875, -230.5495695598654322 ) ) ;
#14715 = CARTESIAN_POINT ( 'NONE',  ( -11.97657177269377371, -18.30092786828533846, -219.1278344157730942 ) ) ;
#14716 = ORIENTED_EDGE ( 'NONE', *, *, #13732, .F. ) ;
#14717 = CARTESIAN_POINT ( 'NONE',  ( -12.43544732248594720, 12.69828336922617318, -219.3367909706387877 ) ) ;
#14718 = CARTESIAN_POINT ( 'NONE',  ( 9.774133712851615030, 11.09751083462123766, -229.6876724410067823 ) ) ;
#14719 = CARTESIAN_POINT ( 'NONE',  ( 2.892356176081334773, 24.03953794589038395, -215.3901262983647200 ) ) ;
#14720 = CARTESIAN_POINT ( 'NONE',  ( -24.95561420934758701, -9.148537957313763513, -219.7769960911953149 ) ) ;
#14721 = DIRECTION ( 'NONE',  ( -1.000000000000000000, 0.000000000000000000, 0.000000000000000000 ) ) ;
#14722 = ORIENTED_EDGE ( 'NONE', *, *, #2230, .F. ) ;
#14723 = CARTESIAN_POINT ( 'NONE',  ( -12.78558550453068854, 7.693178343823584342, -230.0800953344970878 ) ) ;
#14724 = CARTESIAN_POINT ( 'NONE',  ( -7.835169104947472540, -15.11139199849201908, -217.2594261031170220 ) ) ;
#14725 = CYLINDRICAL_SURFACE ( 'NONE', #21616, 25.00000000000010303 ) ;
#14726 = CARTESIAN_POINT ( 'NONE',  ( -3.368164009525018265, 19.03203264544105622, -233.5986411977714567 ) ) ;
#14727 = CARTESIAN_POINT ( 'NONE',  ( 0.000000000000000000, 0.000000000000000000, -78.50000000000000000 ) ) ;
#14728 = CARTESIAN_POINT ( 'NONE',  ( -26.88784739727922357, 10.07520213145270915, -227.1866063047054922 ) ) ;
#14729 = CARTESIAN_POINT ( 'NONE',  ( 8.454338299486085617, 13.28844197278511530, -217.6979371188311632 ) ) ;
#14730 = CARTESIAN_POINT ( 'NONE',  ( 0.000000000000000000, 0.000000000000000000, 75.00000000000000000 ) ) ;
#14731 = CARTESIAN_POINT ( 'NONE',  ( 12.71450444683213021, 7.595266944807587350, -224.4213778964231665 ) ) ;
#14732 = DIRECTION ( 'NONE',  ( 0.000000000000000000, 0.000000000000000000, -1.000000000000000000 ) ) ;
#14733 = CARTESIAN_POINT ( 'NONE',  ( 14.87638776485545122, -7.040696290218329878, -226.6726542491997805 ) ) ;
#14734 = CARTESIAN_POINT ( 'NONE',  ( -13.52935284690462758, -5.503084506376929141, -222.3607690796775671 ) ) ;
#14735 = CARTESIAN_POINT ( 'NONE',  ( 24.99999999999999645, 1.360023205165816762E-13, 0.000000000000000000 ) ) ;
#14736 = CARTESIAN_POINT ( 'NONE',  ( -2.129100187576105530, 26.11057959790866789, -231.5939360033278547 ) ) ;
#14737 = CARTESIAN_POINT ( 'NONE',  ( 31.43562455973156844, -0.2326399569828876968, -228.1442589022926484 ) ) ;
#14738 = CARTESIAN_POINT ( 'NONE',  ( 25.46470895113276711, -14.41152162994631070, -228.1811935238409035 ) ) ;
#14739 = CARTESIAN_POINT ( 'NONE',  ( -14.57944476639264764, 6.129437248167259433, -229.4766146696829310 ) ) ;
#14740 = CARTESIAN_POINT ( 'NONE',  ( 13.86383614057800884, 4.939477956453596441, -219.6543243356308324 ) ) ;
#14741 = CARTESIAN_POINT ( 'NONE',  ( 10.89019654021101857, 23.08162452736882031, -220.1893104909416934 ) ) ;
#14742 = VERTEX_POINT ( 'NONE', #12649 ) ;
#14743 = CARTESIAN_POINT ( 'NONE',  ( 11.19883971596842720, -26.43874323075700161, -218.8478122585937626 ) ) ;
#14744 = DIRECTION ( 'NONE',  ( 1.000000000000000000, 0.000000000000000000, 0.000000000000000000 ) ) ;
#14745 = CARTESIAN_POINT ( 'NONE',  ( -0.6224962293416278492, 14.12372964796689701, -218.2103911528446645 ) ) ;
#14746 = CARTESIAN_POINT ( 'NONE',  ( 0.1645309800062008665, 15.56029994314186382, -233.1129172884685943 ) ) ;
#14747 = CARTESIAN_POINT ( 'NONE',  ( 26.62161015268053177, -11.01850213254573951, -223.2145259598937344 ) ) ;
#14748 = CARTESIAN_POINT ( 'NONE',  ( -0.1571923090946999446, 19.34188126963334398, -216.6893131123363787 ) ) ;
#14749 = CARTESIAN_POINT ( 'NONE',  ( -0.8583760989383530937, -14.48452571672253697, 93.00000000000001421 ) ) ;
#14750 = CARTESIAN_POINT ( 'NONE',  ( 1.682843645364419993, 12.02583837823347679, -224.9288196625490457 ) ) ;
#14751 = CARTESIAN_POINT ( 'NONE',  ( 26.75877786246624623, 11.80320999550499117, -231.5572967531201414 ) ) ;
#14752 = CARTESIAN_POINT ( 'NONE',  ( -27.82842955277035202, 11.70195273568964112, -227.9294339757464911 ) ) ;
#14753 = CARTESIAN_POINT ( 'NONE',  ( 17.34727976380017722, 4.822939981779328811, -230.8836217450937909 ) ) ;
#14754 = CARTESIAN_POINT ( 'NONE',  ( 8.179023008129211902, 20.84698146175953681, -218.6376653143925921 ) ) ;
#14755 = CARTESIAN_POINT ( 'NONE',  ( -1.232595164407830946E-29, 17.50000000000007105, -30.00000000000000000 ) ) ;
#14756 = ORIENTED_EDGE ( 'NONE', *, *, #5761, .T. ) ;
#14757 = CARTESIAN_POINT ( 'NONE',  ( 5.446894657575932719, 15.00061806465251557, -226.4498309983864317 ) ) ;
#14758 = CARTESIAN_POINT ( 'NONE',  ( -11.49803752765619258, -8.459563989871591971, -222.4296168992866853 ) ) ;
#14759 = CARTESIAN_POINT ( 'NONE',  ( 14.32085100525799248, 9.220655089380342062, -219.9006227404039464 ) ) ;
#14760 = CARTESIAN_POINT ( 'NONE',  ( -7.534279315020126155, -14.09704863723370494, -220.2840498463326355 ) ) ;
#14761 = DIRECTION ( 'NONE',  ( -1.000000000000000000, 0.000000000000000000, 0.000000000000000000 ) ) ;
#14762 = CARTESIAN_POINT ( 'NONE',  ( -11.94782396647286049, 8.456988817430419303, -225.5094493096559063 ) ) ;
#14763 = LINE ( 'NONE', #2486, #11725 ) ;
#14764 = CARTESIAN_POINT ( 'NONE',  ( 10.08089751255479527, -9.763210684072014089, -226.4220581413412390 ) ) ;
#14765 = CARTESIAN_POINT ( 'NONE',  ( 12.11771628698343051, 17.56545729485151952, -218.0322663566023493 ) ) ;
#14766 = CARTESIAN_POINT ( 'NONE',  ( -13.31590776630363315, 5.340120742929252096, -225.6956515496373186 ) ) ;
#14767 = CARTESIAN_POINT ( 'NONE',  ( -10.59650102373989533, 7.849913810122476576, -230.0486530042683171 ) ) ;
#14768 = CARTESIAN_POINT ( 'NONE',  ( -22.35893676869521229, -6.243268429983856116, -219.2540196962538062 ) ) ;
#14769 = CONICAL_SURFACE ( 'NONE', #8706, 23.03038449397558196, 0.1745329251994333364 ) ;
#14770 = EDGE_CURVE ( 'NONE', #16045, #17384, #18351, .T. ) ;
#14771 = CARTESIAN_POINT ( 'NONE',  ( 11.50837930502119733, 10.86662242793286381, -233.1728506169798436 ) ) ;
#14772 = CARTESIAN_POINT ( 'NONE',  ( -25.00000000000013500, 6.609496070381316956E-17, -10.00000000000000000 ) ) ;
#14773 = CARTESIAN_POINT ( 'NONE',  ( -23.43110653090080930, -15.10372739875494297, -233.3642232949313211 ) ) ;
#14774 = CARTESIAN_POINT ( 'NONE',  ( 7.450672702945051462, 17.42371045663376705, -217.2894981592719432 ) ) ;
#14775 = CARTESIAN_POINT ( 'NONE',  ( 23.21336156720804667, 12.57464006230432574, -232.9346648124233070 ) ) ;
#14776 = CARTESIAN_POINT ( 'NONE',  ( -11.79656379827575918, 10.43402410864828589, -226.0519616335988076 ) ) ;
#14777 = EDGE_CURVE ( 'NONE', #15721, #12453, #5909, .T. ) ;
#14778 = CARTESIAN_POINT ( 'NONE',  ( 17.88619020626327938, 19.43517936004721847, -216.7078103882350604 ) ) ;
#14779 = CARTESIAN_POINT ( 'NONE',  ( -1.602612909676673469, -20.69807258397210248, -232.3153362903766492 ) ) ;
#14780 = CARTESIAN_POINT ( 'NONE',  ( -6.749503758482277682, -23.22604375411988187, -218.1095993038993299 ) ) ;
#14781 = CARTESIAN_POINT ( 'NONE',  ( -11.10543627608095285, 3.497967533612860613, -224.1342318769322617 ) ) ;
#14782 = CARTESIAN_POINT ( 'NONE',  ( 22.14341918773124362, -7.622004812940091689, -217.4502831791021720 ) ) ;
#14783 = ADVANCED_FACE ( 'NONE', ( #21183 ), #7722, .T. ) ;
#14784 = CARTESIAN_POINT ( 'NONE',  ( -23.14980455159086503, 0.3541108476526578785, -217.8785187302087536 ) ) ;
#14785 = CARTESIAN_POINT ( 'NONE',  ( -15.17658589853145479, -26.64966442869902252, -226.8090782225333442 ) ) ;
#14786 = CARTESIAN_POINT ( 'NONE',  ( 8.321021197036545303, 25.59447019508656140, -228.6184429848799482 ) ) ;
#14787 = CARTESIAN_POINT ( 'NONE',  ( 16.26115440404298340, 3.800605480264513059, -219.2833057824682612 ) ) ;
#14788 = CARTESIAN_POINT ( 'NONE',  ( 5.141746912158045468, 22.01688500372448232, -216.6678693612369386 ) ) ;
#14789 = CARTESIAN_POINT ( 'NONE',  ( 3.241594727517011609, 27.64703009302456138, -225.5540025036233374 ) ) ;
#14790 = CARTESIAN_POINT ( 'NONE',  ( 10.16297913136807907, -22.49776018550796408, -215.0507767410722977 ) ) ;
#14791 = CARTESIAN_POINT ( 'NONE',  ( 11.98894270675143225, 20.38243841428667835, -233.2283128908360084 ) ) ;
#14792 = CARTESIAN_POINT ( 'NONE',  ( -15.47996233766743934, 8.203483081506188768, -221.0931279926996353 ) ) ;
#14793 = CARTESIAN_POINT ( 'NONE',  ( -19.35155980425159683, 1.157993580480985552, -230.3698774940947942 ) ) ;
#14794 = CARTESIAN_POINT ( 'NONE',  ( -7.084830653876206696, -25.45310193036084456, -219.3007580301989492 ) ) ;
#14795 = CARTESIAN_POINT ( 'NONE',  ( 0.000000000000000000, 0.000000000000000000, -55.00000000000000000 ) ) ;
#14796 = CARTESIAN_POINT ( 'NONE',  ( 0.000000000000000000, 24.63401512838747820, 77.51594804401857175 ) ) ;
#14797 = AXIS2_PLACEMENT_3D ( 'NONE', #18865, #20313, #15057 ) ;
#14798 = CARTESIAN_POINT ( 'NONE',  ( 14.31308345469695453, 12.76656023072872159, -231.9445021321040770 ) ) ;
#14799 = CARTESIAN_POINT ( 'NONE',  ( 16.44812011099018889, -8.334251478664654655, -229.6488175962812761 ) ) ;
#14800 = CARTESIAN_POINT ( 'NONE',  ( -29.16153046926437753, 6.356672163541281506, -226.4393515956758165 ) ) ;
#14801 = CARTESIAN_POINT ( 'NONE',  ( -15.62091161899253855, -26.00636881980398840, -222.1463585103649905 ) ) ;
#14802 = APPLICATION_PROTOCOL_DEFINITION ( 'draft international standard', 'automotive_design', 1998, #5984 ) ;
#14803 = CARTESIAN_POINT ( 'NONE',  ( 4.656903975822286768, 13.45000048768594780, -227.6722060245555497 ) ) ;
#14804 = CIRCLE ( 'NONE', #11567, 22.96914677622851642 ) ;
#14805 = CARTESIAN_POINT ( 'NONE',  ( -4.296082356836364191, 12.57880442405704002, -229.5247240216588125 ) ) ;
#14806 = EDGE_LOOP ( 'NONE', ( #281, #4899, #12698, #19018, #12224, #7442, #10160, #3743, #19184, #5704, #868, #20336, #18819, #21016, #1112, #2748, #13910, #22231, #17181, #5816, #8658, #4039, #15519, #99, #21103, #12788 ) ) ;
#14807 = CARTESIAN_POINT ( 'NONE',  ( -3.368164009525018265, 19.03203264544105622, -233.5986411977714567 ) ) ;
#14808 = CARTESIAN_POINT ( 'NONE',  ( -15.92941692657317354, -7.780888323563449838, -232.0381278758927976 ) ) ;
#14809 = CARTESIAN_POINT ( 'NONE',  ( -25.00000000000000000, -1.002884296170500229E-19, 10.00000000000000000 ) ) ;
#14810 = CARTESIAN_POINT ( 'NONE',  ( 1.387778780781446180E-13, -19.80000000000006111, 78.50000000000000000 ) ) ;
#14811 = CARTESIAN_POINT ( 'NONE',  ( -17.75316132689678383, 25.03468689048078843, -222.1645193425721061 ) ) ;
#14812 = CARTESIAN_POINT ( 'NONE',  ( -7.274850400134849515, -18.40080456867533698, -234.8703629377345692 ) ) ;
#14813 = CARTESIAN_POINT ( 'NONE',  ( 23.44296991241933981, -12.51566675729016964, -231.4065378011870564 ) ) ;
#14814 = CARTESIAN_POINT ( 'NONE',  ( -10.24288955603410933, 28.30762631303078791, -220.8855665231519083 ) ) ;
#14815 = AXIS2_PLACEMENT_3D ( 'NONE', #8266, #6566, #10478 ) ;
#14816 = CARTESIAN_POINT ( 'NONE',  ( -19.59898341672158040, 3.279988180491820504, -234.9371679595475086 ) ) ;
#14817 = CARTESIAN_POINT ( 'NONE',  ( -1.582540545905128049, 14.52388882916313584, -222.9138157219475147 ) ) ;
#14818 = CARTESIAN_POINT ( 'NONE',  ( -18.71530386740073126, -0.6857509888707814527, -217.6195632122020527 ) ) ;
#14819 = CARTESIAN_POINT ( 'NONE',  ( 15.33128967029630729, 6.504525012335983902, -229.0514072561169883 ) ) ;
#14820 = CARTESIAN_POINT ( 'NONE',  ( -13.27091111731893847, -21.09541201825366841, -219.8810390191036106 ) ) ;
#14821 = ORIENTED_EDGE ( 'NONE', *, *, #17961, .T. ) ;
#14822 = CARTESIAN_POINT ( 'NONE',  ( -19.74163224554151697, 8.726897413558679872, -232.6665747339030190 ) ) ;
#14823 = CARTESIAN_POINT ( 'NONE',  ( 14.20064147608437821, 14.63411858269657806, -233.6150408276221242 ) ) ;
#14824 = CARTESIAN_POINT ( 'NONE',  ( -0.7286890422672397394, 21.00519367000705273, -234.2149015821977969 ) ) ;
#14825 = TOROIDAL_SURFACE ( 'NONE', #14112, 22.63401512838748175, 3.000000000000002665 ) ;
#14826 = CARTESIAN_POINT ( 'NONE',  ( 24.68983475587330645, -0.6584631617853404784, -233.6195837498767958 ) ) ;
#14827 = DIRECTION ( 'NONE',  ( 0.000000000000000000, 0.000000000000000000, -1.000000000000000000 ) ) ;
#14828 = ORIENTED_EDGE ( 'NONE', *, *, #15458, .F. ) ;
#14829 = CARTESIAN_POINT ( 'NONE',  ( -21.02719846458807851, 18.12262440796364871, -218.0220709499931502 ) ) ;
#14830 = CARTESIAN_POINT ( 'NONE',  ( -19.56933409648781108, -21.97186532644649759, -218.6835957583845982 ) ) ;
#14831 = CARTESIAN_POINT ( 'NONE',  ( 20.89184612657454920, 5.404957034965973683, -232.0952743654565609 ) ) ;
#14832 = CARTESIAN_POINT ( 'NONE',  ( 8.812073984913094904, 13.12649198322903210, -229.9172071780580495 ) ) ;
#14833 = DIRECTION ( 'NONE',  ( -1.000000000000000000, 0.000000000000000000, 0.000000000000000000 ) ) ;
#14834 = PRODUCT_DEFINITION_CONTEXT ( 'detailed design', #14477, 'design' ) ;
#14835 = CARTESIAN_POINT ( 'NONE',  ( -11.59479561055411345, 9.544396733298208702, -229.1494558965577255 ) ) ;
#14836 = VECTOR ( 'NONE', #16727, 1000.000000000000000 ) ;
#14837 = CARTESIAN_POINT ( 'NONE',  ( 9.533850545951205291, 16.09136358716069637, -215.9093469876620475 ) ) ;
#14838 = AXIS2_PLACEMENT_3D ( 'NONE', #19233, #15981, #8899 ) ;
#14839 = CARTESIAN_POINT ( 'NONE',  ( 14.31543143644129579, 0.1402917260236258845, -222.0030278161239039 ) ) ;
#14840 = CARTESIAN_POINT ( 'NONE',  ( 14.31308345469695453, 12.76656023072872159, -231.9445021321040770 ) ) ;
#14841 = CARTESIAN_POINT ( 'NONE',  ( 0.000000000000000000, 0.000000000000000000, 78.50000000000000000 ) ) ;
#14842 = CARTESIAN_POINT ( 'NONE',  ( 23.43833711860394686, -7.060024820847174531, -230.3984000052215606 ) ) ;
#14843 = CARTESIAN_POINT ( 'NONE',  ( -11.39823187951283501, -7.998194509987097689, -226.8062974464413912 ) ) ;
#14844 = CARTESIAN_POINT ( 'NONE',  ( -22.03110473117843071, -6.610460937067380804, -7.510453512272658116 ) ) ;
#14845 = PLANE ( 'NONE',  #2975 ) ;
#14846 = CARTESIAN_POINT ( 'NONE',  ( -0.7292515499105728383, 28.18841485102515776, -220.8637599502617093 ) ) ;
#14847 = CARTESIAN_POINT ( 'NONE',  ( 22.56961104628404868, -1.854966590244772950, -214.8717168148014025 ) ) ;
#14848 = CARTESIAN_POINT ( 'NONE',  ( 14.90979066288448429, -1.927202206923867234, -222.7790985701595616 ) ) ;
#14849 = CARTESIAN_POINT ( 'NONE',  ( -26.02492405343843984, 6.940268742526972900, -218.8798307745116460 ) ) ;
#14850 = CARTESIAN_POINT ( 'NONE',  ( 18.40125535140034430, 0.01434342441762339639, -233.2485400239426099 ) ) ;
#14851 = CARTESIAN_POINT ( 'NONE',  ( 16.07044873961816123, 22.39643131523411412, -226.8512752114033901 ) ) ;
#14852 = CARTESIAN_POINT ( 'NONE',  ( -0.4481215836501183380, -14.49514564254841353, -225.8120917640279970 ) ) ;
#14853 = DIRECTION ( 'NONE',  ( 1.000000000000000000, 0.000000000000000000, 0.000000000000000000 ) ) ;
#14854 = CIRCLE ( 'NONE', #17731, 5.000000000000000888 ) ;
#14855 = CARTESIAN_POINT ( 'NONE',  ( -14.74212732455322161, 0.2624230007780231633, -231.8143822214177874 ) ) ;
#14856 = CIRCLE ( 'NONE', #20581, 16.02266676603872142 ) ;
#14857 = CARTESIAN_POINT ( 'NONE',  ( 12.46318849118074112, 25.01309605388695445, -216.9820503660967859 ) ) ;
#14858 = CARTESIAN_POINT ( 'NONE',  ( 4.966801760238292118, 27.41406605988239420, -216.4490579899774900 ) ) ;
#14859 = CARTESIAN_POINT ( 'NONE',  ( 25.31834813234691595, -9.473547856983202564, -230.2364162768838298 ) ) ;
#14860 = CARTESIAN_POINT ( 'NONE',  ( 0.6364901924797052857, 13.89978473517355617, -221.8840706290426397 ) ) ;
#14861 = CARTESIAN_POINT ( 'NONE',  ( -20.43618815875133521, 1.403378831510147196, -232.9646741665398224 ) ) ;
#14862 = ADVANCED_FACE ( 'NONE', ( #4084 ), #13473, .T. ) ;
#14863 = CARTESIAN_POINT ( 'NONE',  ( -5.566280468132954518, 29.91920859341914962, -222.2705790733167817 ) ) ;
#14864 = CARTESIAN_POINT ( 'NONE',  ( -15.51814470728089645, 2.949994979016113739, -222.8331727603033130 ) ) ;
#14865 = CARTESIAN_POINT ( 'NONE',  ( -15.48255455842386219, 10.01793346089237069, -233.1197357361336913 ) ) ;
#14866 = CARTESIAN_POINT ( 'NONE',  ( 14.63113973005795643, 4.926264598692385199, -222.4866305912601945 ) ) ;
#14867 = TOROIDAL_SURFACE ( 'NONE', #4796, 24.63401512838747820, 3.000000000000000888 ) ;
#14868 = CARTESIAN_POINT ( 'NONE',  ( 4.044213993247089967, 16.45246633354041421, -227.9255899743332918 ) ) ;
#14869 = TOROIDAL_SURFACE ( 'NONE', #7327, 22.63401512838748175, 3.000000000000002665 ) ;
#14870 = DIRECTION ( 'NONE',  ( 0.000000000000000000, -1.000000000000000000, 0.000000000000000000 ) ) ;
#14871 = DIRECTION ( 'NONE',  ( -1.000000000000000000, 0.000000000000000000, 0.000000000000000000 ) ) ;
#14872 = CARTESIAN_POINT ( 'NONE',  ( 8.132753622789847370, 14.44084924206385701, -222.7013822740049704 ) ) ;
#14873 = CARTESIAN_POINT ( 'NONE',  ( -8.491902988188710921, -10.37035003683405066, -223.9502466269643435 ) ) ;
#14874 = CARTESIAN_POINT ( 'NONE',  ( 14.95414693437772868, 8.262206471704862665, -230.1862972580043163 ) ) ;
#14875 = CARTESIAN_POINT ( 'NONE',  ( -0.1378023845299804762, -12.51091464425689104, -226.1051157421467508 ) ) ;
#14876 = CARTESIAN_POINT ( 'NONE',  ( 21.91438441782059954, 0.08560050869924538952, -222.0000000000000000 ) ) ;
#14877 = CARTESIAN_POINT ( 'NONE',  ( -5.365396334125453137, 16.47374957271378904, -219.4721119688156534 ) ) ;
#14878 = CARTESIAN_POINT ( 'NONE',  ( 21.50885124049339936, -13.38680967545814404, -232.7305552638522954 ) ) ;
#14879 = CARTESIAN_POINT ( 'NONE',  ( 21.27834046766391651, 19.84195992785746654, -221.8454931627593965 ) ) ;
#14880 = CARTESIAN_POINT ( 'NONE',  ( -9.810154340578240095, 25.84808829058669488, -220.5759521898573610 ) ) ;
#14881 = CARTESIAN_POINT ( 'NONE',  ( -10.54177647804913320, 7.401649028325941515, -220.3980514230326264 ) ) ;
#14882 = CARTESIAN_POINT ( 'NONE',  ( -13.04844958635619001, -9.307545681632840129, -223.5508123433884009 ) ) ;
#14883 = CARTESIAN_POINT ( 'NONE',  ( 18.59615491886314231, -0.2392802120807639710, -217.5848846836084078 ) ) ;
#14884 = CIRCLE ( 'NONE', #13818, 22.97235139684061878 ) ;
#14885 = FACE_OUTER_BOUND ( 'NONE', #14375, .T. ) ;
#14886 = EDGE_CURVE ( 'NONE', #19977, #17437, #9520, .T. ) ;
#14887 = CARTESIAN_POINT ( 'NONE',  ( -22.35094797335686678, -23.29487558099128108, -223.4832390375085538 ) ) ;
#14888 = CARTESIAN_POINT ( 'NONE',  ( 11.98894270675143225, 20.38243841428667835, -233.2283128908360084 ) ) ;
#14889 = CIRCLE ( 'NONE', #5165, 17.50000000000000355 ) ;
#14890 = CARTESIAN_POINT ( 'NONE',  ( 30.60340911705754863, 5.703403611927857497, -225.1938343315648297 ) ) ;
#14891 = CARTESIAN_POINT ( 'NONE',  ( -1.406618399933933006, 16.47239985789244443, -232.2564017133012726 ) ) ;
#14892 = CARTESIAN_POINT ( 'NONE',  ( 16.11883106748507188, 21.48229216499086291, -233.4985352728212433 ) ) ;
#14893 = EDGE_CURVE ( 'NONE', #1644, #11119, #2678, .T. ) ;
#14894 = ORIENTED_EDGE ( 'NONE', *, *, #11959, .T. ) ;
#14895 = CARTESIAN_POINT ( 'NONE',  ( -5.577337716965932835, -27.36628652700976971, -219.4670492756933413 ) ) ;
#14896 = VERTEX_POINT ( 'NONE', #500 ) ;
#14897 = CARTESIAN_POINT ( 'NONE',  ( -5.693514143275418604, -18.22526881224050754, -218.3451910747569968 ) ) ;
#14898 = CARTESIAN_POINT ( 'NONE',  ( -28.76901170826145560, 13.32870333992657663, -228.6722616467874616 ) ) ;
#14899 = CARTESIAN_POINT ( 'NONE',  ( 10.99893791904045415, -12.61823049403341201, -218.3266956685045841 ) ) ;
#14900 = CARTESIAN_POINT ( 'NONE',  ( -28.55814054826834791, -1.660722980825670048, -228.2640858091212408 ) ) ;
#14901 = CARTESIAN_POINT ( 'NONE',  ( -14.84823930505322132, -23.35465403802561823, -218.3226235040776260 ) ) ;
#14902 = CARTESIAN_POINT ( 'NONE',  ( 11.75069299018312208, 6.043853022588032253, -224.2604610870103841 ) ) ;
#14903 = CYLINDRICAL_SURFACE ( 'NONE', #14591, 17.50000000000000355 ) ;
#14904 = CARTESIAN_POINT ( 'NONE',  ( -12.39654240422350462, 9.886262337642440556, -219.1620329226848014 ) ) ;
#14905 = CARTESIAN_POINT ( 'NONE',  ( 26.39436175479395885, 14.32821500273865034, -221.6819523832376149 ) ) ;
#14906 = VECTOR ( 'NONE', #4661, 1000.000000000000000 ) ;
#14907 = CARTESIAN_POINT ( 'NONE',  ( -1.881996891245037995, 28.05344686410985489, -218.6379207300106202 ) ) ;
#14908 = CARTESIAN_POINT ( 'NONE',  ( 19.70286159681817750, 17.87637900817293612, -218.6154571368943493 ) ) ;
#14909 = CARTESIAN_POINT ( 'NONE',  ( 8.343550503364536297, -10.95302570107183726, -218.8523668966870446 ) ) ;
#14910 = CARTESIAN_POINT ( 'NONE',  ( 21.52074627118099315, 8.791036694007010155, -215.9547738671300294 ) ) ;
#14911 = CARTESIAN_POINT ( 'NONE',  ( -6.415689407129693045, 29.32186846096819011, -228.3852515614991887 ) ) ;
#14912 = EDGE_CURVE ( 'NONE', #15541, #3431, #5557, .T. ) ;
#14913 = CARTESIAN_POINT ( 'NONE',  ( -8.983992482398329926, -13.08794618741998761, -229.3325301586503713 ) ) ;
#14914 = CARTESIAN_POINT ( 'NONE',  ( -22.47200958260654957, 4.697452857301940732, -216.5879371680706242 ) ) ;
#14915 = DIRECTION ( 'NONE',  ( 0.000000000000000000, -0.7999999999999997113, 0.6000000000000004219 ) ) ;
#14916 = CARTESIAN_POINT ( 'NONE',  ( 23.49048926389013658, 9.645778135078892035, -218.7307869890797463 ) ) ;
#14917 = CARTESIAN_POINT ( 'NONE',  ( 15.34439776706934921, -6.609831973102724412, -222.6284221295667862 ) ) ;
#14918 = DIRECTION ( 'NONE',  ( 0.000000000000000000, 0.000000000000000000, 1.000000000000000000 ) ) ;
#14919 = CARTESIAN_POINT ( 'NONE',  ( -1.633632075387274840, -15.48245080501611071, -218.5193615163172751 ) ) ;
#14920 = CARTESIAN_POINT ( 'NONE',  ( -3.643097910890548796, 22.16888955197135047, -233.9701981029593298 ) ) ;
#14921 = CIRCLE ( 'NONE', #9172, 21.00000000000008171 ) ;
#14922 = CARTESIAN_POINT ( 'NONE',  ( -3.309130212696198559, 28.80211350556483296, -217.4284252357080334 ) ) ;
#14923 = ORIENTED_EDGE ( 'NONE', *, *, #315, .T. ) ;
#14924 = CARTESIAN_POINT ( 'NONE',  ( -3.326157069579807946, 13.92020081821418565, -220.5733722327383930 ) ) ;
#14925 = CARTESIAN_POINT ( 'NONE',  ( -27.06419889410506485, -1.187659473326917237, -217.6367138431444630 ) ) ;
#14926 = MECHANICAL_DESIGN_GEOMETRIC_PRESENTATION_REPRESENTATION (  '', ( #21375 ), #21726 ) ;
#14927 = CARTESIAN_POINT ( 'NONE',  ( -24.49265865991512214, -5.019550820411826209, 8.655126539049678769 ) ) ;
#14928 = CARTESIAN_POINT ( 'NONE',  ( 26.00000000000000000, 1.360023205165816762E-13, -9.000000000000001776 ) ) ;
#14929 = CARTESIAN_POINT ( 'NONE',  ( 5.331555957413248059, 27.50712867803999728, -219.0801070358024276 ) ) ;
#14930 = CARTESIAN_POINT ( 'NONE',  ( -14.63769981573866552, -28.59145599960802642, -226.8825043222271631 ) ) ;
#14931 = CARTESIAN_POINT ( 'NONE',  ( 5.953549895739506326, -12.70069413479034104, -221.3143591192976203 ) ) ;
#14932 = CARTESIAN_POINT ( 'NONE',  ( 17.28140336138120858, -11.48510652344925020, -216.9852223368602893 ) ) ;
#14933 = CARTESIAN_POINT ( 'NONE',  ( -12.27164519775873686, 10.97713184439464840, -231.6269036897678291 ) ) ;
#14934 = CARTESIAN_POINT ( 'NONE',  ( 11.21155440434494643, 24.57152134148167733, -221.7155903571010356 ) ) ;
#14935 = CARTESIAN_POINT ( 'NONE',  ( -24.68906941503829700, 2.445024713909649705, -232.6803430500543755 ) ) ;
#14936 = CARTESIAN_POINT ( 'NONE',  ( -17.18633058961025029, 6.481319267413964802, -216.1357216783315494 ) ) ;
#14937 = CARTESIAN_POINT ( 'NONE',  ( -24.66391263913385856, -10.62169550967977472, -229.5175364317193498 ) ) ;
#14938 = ORIENTED_EDGE ( 'NONE', *, *, #10238, .F. ) ;
#14939 = CARTESIAN_POINT ( 'NONE',  ( -15.36327147092456791, 5.453733681707060299, -220.0043800961136355 ) ) ;
#14940 = CARTESIAN_POINT ( 'NONE',  ( 2.785859284650920031, 14.19821255961969619, -226.9946081512528906 ) ) ;
#14941 = CARTESIAN_POINT ( 'NONE',  ( 2.068961274655788607, 15.13167107497539376, -217.8084559455312501 ) ) ;
#14942 = EDGE_CURVE ( 'NONE', #13805, #19507, #2331, .T. ) ;
#14943 = CARTESIAN_POINT ( 'NONE',  ( -21.75565187119130428, -2.221346625543990427, -217.0768970814220609 ) ) ;
#14944 = DIRECTION ( 'NONE',  ( 0.000000000000000000, 0.000000000000000000, -1.000000000000000000 ) ) ;
#14945 = CIRCLE ( 'NONE', #7396, 17.50000000000001066 ) ;
#14946 = VERTEX_POINT ( 'NONE', #8227 ) ;
#14947 = CIRCLE ( 'NONE', #12783, 2.999999999999999112 ) ;
#14948 = CARTESIAN_POINT ( 'NONE',  ( -10.65455960636934662, 10.37188583052882862, -219.5197110153079620 ) ) ;
#14949 = CARTESIAN_POINT ( 'NONE',  ( -13.74974073587016576, -14.61773948691506142, -215.3128624239759290 ) ) ;
#14950 = CARTESIAN_POINT ( 'NONE',  ( 16.00819137755116373, 4.595691552992191120, -229.5669508871464757 ) ) ;
#14951 = CARTESIAN_POINT ( 'NONE',  ( 10.57926812561479757, 10.00910231482511215, -225.8341706491384286 ) ) ;
#14952 = CARTESIAN_POINT ( 'NONE',  ( 0.000000000000000000, -17.50000000000000711, -55.00000000000000000 ) ) ;
#14953 = CARTESIAN_POINT ( 'NONE',  ( 29.17814965709308694, -1.309718763918959139, -225.2029557489520926 ) ) ;
#14954 = CARTESIAN_POINT ( 'NONE',  ( -19.58639255110637478, 14.91076398872931819, -217.1105532241463720 ) ) ;
#14955 = CARTESIAN_POINT ( 'NONE',  ( 13.89183999136464820, 6.553741795688899252, -220.8646181278399752 ) ) ;
#14956 = CARTESIAN_POINT ( 'NONE',  ( -24.89656853084665400, 2.294499589785194971, -9.738719574107680188 ) ) ;
#14957 = CARTESIAN_POINT ( 'NONE',  ( 14.73698509926073186, 4.443590625350892331, -227.4062002049096236 ) ) ;
#14958 = CARTESIAN_POINT ( 'NONE',  ( 16.49868092868510061, -6.867418253114158766, -220.9302697977882133 ) ) ;
#14959 = VECTOR ( 'NONE', #11557, 1000.000000000000000 ) ;
#14960 = CARTESIAN_POINT ( 'NONE',  ( -20.18470553695442860, -13.13924840112635195, -232.9662461559857718 ) ) ;
#14961 = CARTESIAN_POINT ( 'NONE',  ( -21.30902137360851967, -8.664601116739698128, 5.034284465761014182 ) ) ;
#14962 = DIRECTION ( 'NONE',  ( 0.000000000000000000, 0.000000000000000000, -1.000000000000000000 ) ) ;
#14963 = CARTESIAN_POINT ( 'NONE',  ( -5.298027976154672025, 13.43376398981453157, -220.6333279128949982 ) ) ;
#14964 = CARTESIAN_POINT ( 'NONE',  ( 13.17262855481386374, -26.22572064374609013, -230.8671443076513583 ) ) ;
#14965 = CARTESIAN_POINT ( 'NONE',  ( 14.56914850832129815, -2.041740472307377985, -224.7121590863160350 ) ) ;
#14966 = CARTESIAN_POINT ( 'NONE',  ( -24.79507334250576278, 6.844873424762779379, -218.1074956078844878 ) ) ;
#14967 = CARTESIAN_POINT ( 'NONE',  ( 25.38325563848796662, 11.05100313887457553, -217.8685524735130628 ) ) ;
#14968 = CARTESIAN_POINT ( 'NONE',  ( 15.54095364727189299, 10.52000078266145700, -230.2714373371992735 ) ) ;
#14969 = CARTESIAN_POINT ( 'NONE',  ( 13.44856294975069488, -28.16358066815265460, -226.3235907536142406 ) ) ;
#14970 = CARTESIAN_POINT ( 'NONE',  ( 0.000000000000000000, 0.000000000000000000, -20.00000000000000000 ) ) ;
#14971 = CARTESIAN_POINT ( 'NONE',  ( -25.32262741784088078, 2.623212696197013472, -234.6011982779809841 ) ) ;
#14972 = CARTESIAN_POINT ( 'NONE',  ( 10.46530733675539793, 8.351728317179080818, -222.7431177495969621 ) ) ;
#14973 = CARTESIAN_POINT ( 'NONE',  ( 4.213939275857851108, 16.79797086795582928, -215.8378124706958943 ) ) ;
#14974 = CARTESIAN_POINT ( 'NONE',  ( 29.78177645116457128, -4.041743286679309044, -225.6339783681140432 ) ) ;
#14975 = CARTESIAN_POINT ( 'NONE',  ( -3.673551555920188783, 29.81207051619892923, -228.8770490300152005 ) ) ;
#14976 = CARTESIAN_POINT ( 'NONE',  ( -26.58771759052039485, 5.114955214121561511, -218.2823714869195442 ) ) ;
#14977 = AXIS2_PLACEMENT_3D ( 'NONE', #2705, #9589, #1024 ) ;
#14978 = CARTESIAN_POINT ( 'NONE',  ( 8.681721411120292942, 8.442847255497570202, -228.0516816418615065 ) ) ;
#14979 = CARTESIAN_POINT ( 'NONE',  ( -27.32994399549947673, 3.379920396491164603, -227.9326384921875217 ) ) ;
#14980 = CARTESIAN_POINT ( 'NONE',  ( -10.24288955603410933, 28.30762631303078791, -220.8855665231519083 ) ) ;
#14981 = CARTESIAN_POINT ( 'NONE',  ( 14.95414693437772868, 8.262206471704862665, -230.1862972580043163 ) ) ;
#14982 = CARTESIAN_POINT ( 'NONE',  ( 11.39755372583812587, 20.40856199875060639, -231.2895618162029621 ) ) ;
#14983 = CARTESIAN_POINT ( 'NONE',  ( 17.95694455891925756, -3.510678534943489026, -231.2643001502910067 ) ) ;
#14984 = LINE ( 'NONE', #9171, #15635 ) ;
#14985 = CARTESIAN_POINT ( 'NONE',  ( -22.53818779203657741, -7.663114047788936567, -232.6164956747681458 ) ) ;
#14986 = CARTESIAN_POINT ( 'NONE',  ( 21.35706335192880445, 15.67286272432725092, -219.2578158352350783 ) ) ;
#14987 = CARTESIAN_POINT ( 'NONE',  ( -7.442430984977708164, -13.68264719635657301, -220.8544524341123747 ) ) ;
#14988 = DIRECTION ( 'NONE',  ( -1.000000000000000000, 0.000000000000000000, 0.000000000000000000 ) ) ;
#14989 = CARTESIAN_POINT ( 'NONE',  ( -8.407534899841293097, 16.91942258446019665, -231.3029992963236339 ) ) ;
#14990 = EDGE_CURVE ( 'NONE', #14742, #10586, #14921, .T. ) ;
#14991 =( NAMED_UNIT ( * ) SI_UNIT ( $, .STERADIAN. ) SOLID_ANGLE_UNIT ( ) );
#14992 = CARTESIAN_POINT ( 'NONE',  ( 22.55746627616819566, -14.21542447219996852, -231.9819121152456205 ) ) ;
#14993 = CARTESIAN_POINT ( 'NONE',  ( 24.49559427486850893, 14.86117239466233642, -230.3058416388274736 ) ) ;
#14994 = CARTESIAN_POINT ( 'NONE',  ( -7.284474494690100776, 13.60812129561547046, -227.7414351104868331 ) ) ;
#14995 = CARTESIAN_POINT ( 'NONE',  ( -12.19796877179171446, 17.24929682309303658, -234.5722138766719809 ) ) ;
#14996 = ORIENTED_EDGE ( 'NONE', *, *, #20861, .F. ) ;
#14997 = CARTESIAN_POINT ( 'NONE',  ( -17.01759357405825668, -4.262369086395770168, -221.2289172648622184 ) ) ;
#14998 = CARTESIAN_POINT ( 'NONE',  ( 25.09997929702755926, 1.294103573351435221, -217.0485712200477906 ) ) ;
#14999 = CARTESIAN_POINT ( 'NONE',  ( 0.000000000000000000, 0.000000000000000000, -75.00000000000000000 ) ) ;
#15000 = CARTESIAN_POINT ( 'NONE',  ( -14.05955845762884238, -0.8719634938775207011, -221.0475910153949428 ) ) ;
#15001 = CARTESIAN_POINT ( 'NONE',  ( 15.26539804565921621, 9.309431686815628382, -232.9129599938668207 ) ) ;
#15002 = CARTESIAN_POINT ( 'NONE',  ( -25.20870746202117729, 11.68425842440532136, -223.9066764530103342 ) ) ;
#15003 = CARTESIAN_POINT ( 'NONE',  ( 11.31331191788792623, 29.23420701778062281, -220.7538464529627333 ) ) ;
#15004 = CARTESIAN_POINT ( 'NONE',  ( 11.00045714400293306, 20.20239058357963913, -215.1666500215986275 ) ) ;
#15005 = ORIENTED_EDGE ( 'NONE', *, *, #10094, .T. ) ;
#15006 = CARTESIAN_POINT ( 'NONE',  ( -6.241914139598351952, -12.26321662989467320, -220.9276712261616353 ) ) ;
#15007 = ORIENTED_EDGE ( 'NONE', *, *, #11475, .T. ) ;
#15008 = CARTESIAN_POINT ( 'NONE',  ( 6.679827377097204533, -23.59744646493245668, -231.8618301756397670 ) ) ;
#15009 = CARTESIAN_POINT ( 'NONE',  ( -26.12939716039095117, 11.33146045174629357, -233.1192402782019997 ) ) ;
#15010 = CARTESIAN_POINT ( 'NONE',  ( 17.01060404384151781, -6.151862203644831162, -218.3248062500343849 ) ) ;
#15011 = CARTESIAN_POINT ( 'NONE',  ( 27.20328812258980378, -0.4806365347271125965, -218.3128023695579998 ) ) ;
#15012 = CARTESIAN_POINT ( 'NONE',  ( -28.46519324992292965, -8.397260794665152517, -225.6705986409035347 ) ) ;
#15013 = CARTESIAN_POINT ( 'NONE',  ( 20.54489901492447501, 10.52141067440427591, -216.2005526543161693 ) ) ;
#15014 = CARTESIAN_POINT ( 'NONE',  ( -23.00000000000000355, 0.000000000000000000, -75.00000000000000000 ) ) ;
#15015 = CARTESIAN_POINT ( 'NONE',  ( -20.04070223234628756, 18.12164545743767263, -231.9292141396248610 ) ) ;
#15016 = CARTESIAN_POINT ( 'NONE',  ( 12.55473222622303986, 11.30320364856893001, -218.8964119182764989 ) ) ;
#15017 = CARTESIAN_POINT ( 'NONE',  ( 0.9908753270255351575, 13.79205759140780430, -228.0165926715089881 ) ) ;
#15018 = CARTESIAN_POINT ( 'NONE',  ( 9.425340689562565544, 25.38932416188112384, -221.3391712389563963 ) ) ;
#15019 = CARTESIAN_POINT ( 'NONE',  ( 10.25809576580632232, -7.052396458808492419, -221.5466685117269208 ) ) ;
#15020 = CARTESIAN_POINT ( 'NONE',  ( -21.75607741976026333, 20.26169853110213381, -228.4128163609909450 ) ) ;
#15021 = CARTESIAN_POINT ( 'NONE',  ( -0.9851030586975465519, 19.34066537597387381, -233.8273485600932418 ) ) ;
#15022 = CARTESIAN_POINT ( 'NONE',  ( -13.55429797312971374, -24.97278848321653300, -221.1627755146857908 ) ) ;
#15023 = CARTESIAN_POINT ( 'NONE',  ( -21.89065952084848021, -0.9940043559354364566, -216.9999999999999716 ) ) ;
#15024 = CARTESIAN_POINT ( 'NONE',  ( -23.00000000000009237, 0.000000000000000000, 75.00000000000000000 ) ) ;
#15025 = EDGE_CURVE ( 'NONE', #14043, #9939, #5198, .T. ) ;
#15026 = CARTESIAN_POINT ( 'NONE',  ( 15.76910524310159900, 5.601482066865847820, -220.3440822020379528 ) ) ;
#15027 = CARTESIAN_POINT ( 'NONE',  ( 7.829076659910394476, -15.59360078984655651, -230.7142312655459762 ) ) ;
#15028 = CARTESIAN_POINT ( 'NONE',  ( -20.47640197314466093, 18.50423766437512541, -220.4440130802851456 ) ) ;
#15029 = CARTESIAN_POINT ( 'NONE',  ( -0.9249541874382023465, 14.55235618511626328, -223.7321818898853962 ) ) ;
#15030 = CARTESIAN_POINT ( 'NONE',  ( -25.61235545225478560, -15.41032726095661509, -226.9890212492312855 ) ) ;
#15031 = CARTESIAN_POINT ( 'NONE',  ( 29.89309326230132058, 6.052383583152112223, -228.3539431708548477 ) ) ;
#15032 = CARTESIAN_POINT ( 'NONE',  ( 14.65697969206133067, 11.40587726087447606, -233.3943609825344652 ) ) ;
#15033 = ORIENTED_EDGE ( 'NONE', *, *, #627, .F. ) ;
#15034 = CARTESIAN_POINT ( 'NONE',  ( -2.817219543927646175, 14.13981714106644993, -229.6779615865167443 ) ) ;
#15035 = CARTESIAN_POINT ( 'NONE',  ( 15.06969459085678942, -9.685035337269850331, -230.1890524597188801 ) ) ;
#15036 = CARTESIAN_POINT ( 'NONE',  ( -23.91245210406065524, -7.297367535069414934, 6.844934202459222128 ) ) ;
#15037 = DIRECTION ( 'NONE',  ( -0.000000000000000000, -0.000000000000000000, -1.000000000000000000 ) ) ;
#15038 = CARTESIAN_POINT ( 'NONE',  ( 2.837900457371055563, 25.11342719071438978, -232.9871906064174709 ) ) ;
#15039 = CARTESIAN_POINT ( 'NONE',  ( -3.456580335739853016, -11.82839499582713749, -226.8096787805597501 ) ) ;
#15040 = CARTESIAN_POINT ( 'NONE',  ( 13.99926435381047618, -21.11851526759364006, -232.9234173943665951 ) ) ;
#15041 = CARTESIAN_POINT ( 'NONE',  ( 20.80196158924851701, -7.261721507697286526, -217.3074963141844194 ) ) ;
#15042 = CARTESIAN_POINT ( 'NONE',  ( -12.39654240422350462, 9.886262337642440556, -219.1620329226848014 ) ) ;
#15043 = CARTESIAN_POINT ( 'NONE',  ( 11.73428189025226942, 12.46434742632455084, -228.1539301014595083 ) ) ;
#15044 = CARTESIAN_POINT ( 'NONE',  ( -13.92046207272054303, -0.1600067567908077248, -224.5811699126800818 ) ) ;
#15045 = CARTESIAN_POINT ( 'NONE',  ( -21.72273972318264867, 21.08396222359856864, -224.0477214759881690 ) ) ;
#15046 = CARTESIAN_POINT ( 'NONE',  ( -14.19990609618026056, -7.901335420714983293, -227.4892254059333823 ) ) ;
#15047 = ORIENTED_EDGE ( 'NONE', *, *, #11743, .F. ) ;
#15048 = CARTESIAN_POINT ( 'NONE',  ( -11.03778527004271659, 26.96286968643956428, -225.4057095641571209 ) ) ;
#15049 = CARTESIAN_POINT ( 'NONE',  ( 13.48097272627202159, 8.509510470709432894, -231.5257201610278059 ) ) ;
#15050 = CARTESIAN_POINT ( 'NONE',  ( -4.974038791218384326, 28.61915055369004079, -219.5057940952933961 ) ) ;
#15051 = VECTOR ( 'NONE', #1650, 1000.000000000000000 ) ;
#15052 = CARTESIAN_POINT ( 'NONE',  ( 20.07985072697885442, -15.33367264652052953, -217.4666949641080294 ) ) ;
#15053 = CARTESIAN_POINT ( 'NONE',  ( 0.000000000000000000, 0.000000000000000000, -120.0000000000000142 ) ) ;
#15054 = VERTEX_POINT ( 'NONE', #20576 ) ;
#15055 = CARTESIAN_POINT ( 'NONE',  ( -16.65698539163286540, 11.03290537638306112, -233.6474915129378758 ) ) ;
#15056 = CARTESIAN_POINT ( 'NONE',  ( -10.39490437715664228, -5.549361993742060406, -223.4983083630424403 ) ) ;
#15057 = DIRECTION ( 'NONE',  ( 0.000000000000000000, 0.000000000000000000, 1.000000000000000000 ) ) ;
#15058 = CARTESIAN_POINT ( 'NONE',  ( 7.995304978256253747, 13.28024228361502779, -220.6535174700288451 ) ) ;
#15059 = CARTESIAN_POINT ( 'NONE',  ( 0.000000000000000000, 22.63401512838748175, 77.51594804401857175 ) ) ;
#15060 = CARTESIAN_POINT ( 'NONE',  ( 28.52058947142581502, -1.755848367977142610, -221.9695116608532715 ) ) ;
#15061 =( NAMED_UNIT ( * ) PLANE_ANGLE_UNIT ( ) SI_UNIT ( $, .RADIAN. ) );
#15062 = CARTESIAN_POINT ( 'NONE',  ( -16.20072894238734307, 0.5024448614660336210, -230.4554067149722130 ) ) ;
#15063 = CARTESIAN_POINT ( 'NONE',  ( -19.61183938075907918, 22.25855138946451106, -229.5731876748794207 ) ) ;
#15064 = CARTESIAN_POINT ( 'NONE',  ( 24.32561047128371001, 1.769413244618101011, -218.8629106451077462 ) ) ;
#15065 = FILL_AREA_STYLE ('',( #4466 ) ) ;
#15066 = CARTESIAN_POINT ( 'NONE',  ( -24.99323045272601007, 0.6685402709427104018, -9.983109981726205007 ) ) ;
#15067 = EDGE_CURVE ( 'NONE', #10545, #4564, #5164, .T. ) ;
#15068 = LINE ( 'NONE', #19315, #12734 ) ;
#15069 = VECTOR ( 'NONE', #11118, 1000.000000000000000 ) ;
#15070 = CARTESIAN_POINT ( 'NONE',  ( -20.43618815875133521, 1.403378831510147196, -232.9646741665398224 ) ) ;
#15071 = CARTESIAN_POINT ( 'NONE',  ( 16.16137015560671131, -6.751010448487875237, -221.3181884246570519 ) ) ;
#15072 = CARTESIAN_POINT ( 'NONE',  ( -18.89430729770302975, -12.42271633246521212, -233.2230176520695295 ) ) ;
#15073 = EDGE_CURVE ( 'NONE', #351, #15638, #15325, .T. ) ;
#15074 = CARTESIAN_POINT ( 'NONE',  ( 0.000000000000000000, 0.000000000000000000, -77.51594804401857175 ) ) ;
#15075 = CARTESIAN_POINT ( 'NONE',  ( 0.000000000000000000, 0.000000000000000000, -65.00000000000000000 ) ) ;
#15076 = CARTESIAN_POINT ( 'NONE',  ( 2.208705534715813101, 15.26926593729510984, -227.3643075380122980 ) ) ;
#15077 = EDGE_CURVE ( 'NONE', #11287, #22159, #15998, .T. ) ;
#15078 = CARTESIAN_POINT ( 'NONE',  ( 11.27265965248755819, -10.15440342946296148, -217.7707216267749573 ) ) ;
#15079 = CARTESIAN_POINT ( 'NONE',  ( 13.04434844185555420, -10.19049307777131297, -230.8679447648462713 ) ) ;
#15080 = CARTESIAN_POINT ( 'NONE',  ( -20.57288920227272655, 16.51351902378409520, -230.8484733908063333 ) ) ;
#15081 = CARTESIAN_POINT ( 'NONE',  ( 20.10109416526603709, 2.018147939476731434, -216.1034161917718848 ) ) ;
#15082 = CARTESIAN_POINT ( 'NONE',  ( 17.32394486779715592, 4.028159306070694612, -218.4253989884176690 ) ) ;
#15083 = VERTEX_POINT ( 'NONE', #20126 ) ;
#15084 = CARTESIAN_POINT ( 'NONE',  ( -7.461655027780660809, -14.63259296063595727, -227.5661480528262075 ) ) ;
#15085 = CARTESIAN_POINT ( 'NONE',  ( -14.50030254718125100, 0.06328415631827216670, 93.00000000000005684 ) ) ;
#15086 = CARTESIAN_POINT ( 'NONE',  ( -27.68973657932738064, 5.930811633061950694, -216.7842770206311513 ) ) ;
#15087 = CARTESIAN_POINT ( 'NONE',  ( 17.10545320562996352, 22.53742678899184781, -232.4605876935045785 ) ) ;
#15088 = CARTESIAN_POINT ( 'NONE',  ( -1.584125552723561592, 20.48724127025963782, -214.7515060525244621 ) ) ;
#15089 = CARTESIAN_POINT ( 'NONE',  ( 16.69326964758149856, -4.763004462669847783, -219.2590076381798951 ) ) ;
#15090 = CARTESIAN_POINT ( 'NONE',  ( -10.84997096467605182, 25.01800101807719301, -232.4518260228253155 ) ) ;
#15091 = CARTESIAN_POINT ( 'NONE',  ( -16.63766460830045091, 5.158675778507696208, -232.1659425527909093 ) ) ;
#15092 = CARTESIAN_POINT ( 'NONE',  ( 10.85325209735074559, 11.82487774067193342, -216.5214842375702062 ) ) ;
#15093 = CARTESIAN_POINT ( 'NONE',  ( -16.40443871513620522, 4.023423476741658789, -228.9829044427089002 ) ) ;
#15094 = CARTESIAN_POINT ( 'NONE',  ( -8.966714183099560032, 19.05224306381768073, -234.0879867025980445 ) ) ;
#15095 = CARTESIAN_POINT ( 'NONE',  ( 17.07668571305246985, 2.037405138410691485, -219.7626854147787867 ) ) ;
#15096 = CARTESIAN_POINT ( 'NONE',  ( 15.56183105618911355, 23.93598532278018354, -223.2746693648072664 ) ) ;
#15097 = CARTESIAN_POINT ( 'NONE',  ( 14.50000000000000000, 0.000000000000000000, 92.50000000000000000 ) ) ;
#15098 = CARTESIAN_POINT ( 'NONE',  ( 26.00000000000000000, 1.372269673157290277E-13, -10.00000000000000000 ) ) ;
#15099 = CARTESIAN_POINT ( 'NONE',  ( 0.000000000000000000, 0.000000000000000000, -99.99999999999998579 ) ) ;
#15100 = CARTESIAN_POINT ( 'NONE',  ( -16.99821283087967672, -0.5135051709387361552, -216.2173766440975555 ) ) ;
#15101 = CARTESIAN_POINT ( 'NONE',  ( -14.93311267495276518, -24.05029333330348251, -229.1587772033057888 ) ) ;
#15102 = CARTESIAN_POINT ( 'NONE',  ( 21.13193872423781272, 0.8515989525826543893, -227.8817869685189237 ) ) ;
#15103 = CARTESIAN_POINT ( 'NONE',  ( -7.240690404266621805, 13.01623002570985044, -225.3000933658701967 ) ) ;
#15104 = CARTESIAN_POINT ( 'NONE',  ( 7.045253012492558753, -17.38872841331140862, -218.3726031779064556 ) ) ;
#15105 = CARTESIAN_POINT ( 'NONE',  ( 10.98110116949302828, 13.70618071521442971, -230.2797640191687378 ) ) ;
#15106 = CARTESIAN_POINT ( 'NONE',  ( -9.661739055621840322, 20.41227307912577871, -232.0920144483423257 ) ) ;
#15107 = CARTESIAN_POINT ( 'NONE',  ( -7.399925907206128528, 10.29859031525428037, -227.1614041762800298 ) ) ;
#15108 = VERTEX_POINT ( 'NONE', #20352 ) ;
#15109 = CARTESIAN_POINT ( 'NONE',  ( -24.24026017931571175, -14.11860166261188354, -224.3835235244768569 ) ) ;
#15110 = CARTESIAN_POINT ( 'NONE',  ( 7.639528166734322667, 11.92751229241157596, -224.6077814063189635 ) ) ;
#15111 = CARTESIAN_POINT ( 'NONE',  ( 22.69522586737246783, 3.669837464059151344, -234.0947686933411944 ) ) ;
#15112 = DIRECTION ( 'NONE',  ( 1.000000000000000000, 0.000000000000000000, 0.000000000000000000 ) ) ;
#15113 = CARTESIAN_POINT ( 'NONE',  ( -22.24434812881145618, 2.221346625544017961, -216.9231029185778254 ) ) ;
#15114 = CARTESIAN_POINT ( 'NONE',  ( 11.43247012502872728, 12.44034019618676190, -231.9336559008378629 ) ) ;
#15115 = CARTESIAN_POINT ( 'NONE',  ( -16.56270003954679382, 4.935922114544952777, -221.6503923146493378 ) ) ;
#15116 = CARTESIAN_POINT ( 'NONE',  ( 3.711349367426693746, 16.84755988915346236, -233.7359972593521888 ) ) ;
#15117 = CARTESIAN_POINT ( 'NONE',  ( 15.46952826979347151, 3.173892190046953665, -221.7237849701489552 ) ) ;
#15118 = CARTESIAN_POINT ( 'NONE',  ( -17.92393051735373888, -14.45097846726422830, -234.9711082062119374 ) ) ;
#15119 = ORIENTED_EDGE ( 'NONE', *, *, #4223, .F. ) ;
#15120 = CARTESIAN_POINT ( 'NONE',  ( -15.28220591200235390, -15.65475725988279443, -217.1155325995422913 ) ) ;
#15121 = CARTESIAN_POINT ( 'NONE',  ( -13.63292518690856170, 3.968236334994402981, -218.3158317831635316 ) ) ;
#15122 = CARTESIAN_POINT ( 'NONE',  ( 7.486336813247038258, -29.35413437595724773, -221.4114973598149447 ) ) ;
#15123 = CARTESIAN_POINT ( 'NONE',  ( 17.05764047735875266, -11.29112887239367424, -214.9748062598841898 ) ) ;
#15124 = CARTESIAN_POINT ( 'NONE',  ( -26.07210576407111446, -8.413030596423759278, -230.6002792590230115 ) ) ;
#15125 = CARTESIAN_POINT ( 'NONE',  ( 16.97369223523349646, 15.19068754808448851, -217.0779026324121332 ) ) ;
#15126 = CARTESIAN_POINT ( 'NONE',  ( -21.80000000000000071, 0.000000000000000000, 78.50000000000000000 ) ) ;
#15127 = CARTESIAN_POINT ( 'NONE',  ( -13.30451247859013897, 19.85560227862636040, -232.3493821534129609 ) ) ;
#15128 = CARTESIAN_POINT ( 'NONE',  ( 20.85755584069816493, 20.53615333921957742, -227.2010381488614996 ) ) ;
#15129 = CARTESIAN_POINT ( 'NONE',  ( 20.41153371889344825, 17.18812948447019551, -230.7531656956970778 ) ) ;
#15130 = CARTESIAN_POINT ( 'NONE',  ( 10.59524789654300925, 9.532374763983630928, -223.0758647391057821 ) ) ;
#15131 = CARTESIAN_POINT ( 'NONE',  ( 18.64433268355766415, -12.21264687082605782, -214.8850304513305502 ) ) ;
#15132 = CARTESIAN_POINT ( 'NONE',  ( -4.974038791218384326, 28.61915055369004079, -219.5057940952933961 ) ) ;
#15133 = DIRECTION ( 'NONE',  ( -1.000000000000000000, 0.000000000000000000, 0.000000000000000000 ) ) ;
#15134 = DIRECTION ( 'NONE',  ( 1.000000000000000000, 0.000000000000000000, -0.000000000000000000 ) ) ;
#15135 = CARTESIAN_POINT ( 'NONE',  ( 12.23063869552301242, 12.84118223717021934, -218.8273164334868284 ) ) ;
#15136 = CARTESIAN_POINT ( 'NONE',  ( 15.76600796393256410, -24.40864267010898558, -225.5036181134576907 ) ) ;
#15137 = CARTESIAN_POINT ( 'NONE',  ( -22.24722865165759345, 18.77558306771206986, -226.5077042908023941 ) ) ;
#15138 = CARTESIAN_POINT ( 'NONE',  ( -3.223980134944351317, 26.83284996841001302, -219.5167893230652965 ) ) ;
#15139 = CARTESIAN_POINT ( 'NONE',  ( -21.63546480557098306, -21.44004028177477750, -223.8762611443524122 ) ) ;
#15140 = CONTEXT_DEPENDENT_SHAPE_REPRESENTATION ( #16344, #5092 ) ;
#15141 = CARTESIAN_POINT ( 'NONE',  ( 30.60340911705754863, 5.703403611927857497, -225.1938343315648297 ) ) ;
#15142 = CARTESIAN_POINT ( 'NONE',  ( 21.92281339924938877, 16.67475415235398017, -231.9828670874568957 ) ) ;
#15143 = ORIENTED_EDGE ( 'NONE', *, *, #6802, .T. ) ;
#15144 = CARTESIAN_POINT ( 'NONE',  ( 5.343558017910363667, 26.29639771561252459, -218.1010331760174665 ) ) ;
#15145 = CARTESIAN_POINT ( 'NONE',  ( 16.71284463105542883, -8.832875790685479345, -219.1937169315102949 ) ) ;
#15146 = CARTESIAN_POINT ( 'NONE',  ( 12.99512476935412231, -3.120572961704727977, -223.7636045402963987 ) ) ;
#15147 = DIRECTION ( 'NONE',  ( -1.000000000000000000, 0.000000000000000000, 0.000000000000000000 ) ) ;
#15148 = CARTESIAN_POINT ( 'NONE',  ( 5.069241901512100412, 14.34986542013820632, -229.6420000777802954 ) ) ;
#15149 = CARTESIAN_POINT ( 'NONE',  ( -27.52442056016948868, -15.72718643249855397, -222.0944556419597689 ) ) ;
#15150 = CARTESIAN_POINT ( 'NONE',  ( 11.32394539683753720, -15.63383003174572572, -233.0723040138117881 ) ) ;
#15151 = CARTESIAN_POINT ( 'NONE',  ( 15.10937218716165020, -26.44221868192832758, -222.7999243300199907 ) ) ;
#15152 = CARTESIAN_POINT ( 'NONE',  ( -9.734169867326336600, 14.53420431798807755, -231.2442251076483046 ) ) ;
#15153 = CARTESIAN_POINT ( 'NONE',  ( 13.96918721733258195, 14.12724320058294403, -230.4946432816737172 ) ) ;
#15154 = CARTESIAN_POINT ( 'NONE',  ( -15.15110768032078070, 3.517015312212880218, -219.5479300368539270 ) ) ;
#15155 = CARTESIAN_POINT ( 'NONE',  ( -29.98527381603928887, 6.316825171121390525, -230.1108345570740994 ) ) ;
#15156 = CARTESIAN_POINT ( 'NONE',  ( -16.02921639098982709, -5.689335215210093999, -220.0011032104688979 ) ) ;
#15157 = ORIENTED_EDGE ( 'NONE', *, *, #14233, .F. ) ;
#15158 = CARTESIAN_POINT ( 'NONE',  ( -8.030397104878142400, 15.90963402996711373, -230.6518438502475590 ) ) ;
#15159 = CARTESIAN_POINT ( 'NONE',  ( 19.40629804599390340, 15.10110417999774057, -216.3942729496570223 ) ) ;
#15160 = CARTESIAN_POINT ( 'NONE',  ( -0.9851030586975465519, 19.34066537597387381, -233.8273485600932418 ) ) ;
#15161 = CARTESIAN_POINT ( 'NONE',  ( 24.96165930385824794, -17.14663603160204275, -224.2745859498249672 ) ) ;
#15162 = CYLINDRICAL_SURFACE ( 'NONE', #5684, 10.00000000000000000 ) ;
#15163 = EDGE_LOOP ( 'NONE', ( #2443, #349, #9127, #1841 ) ) ;
#15164 = CARTESIAN_POINT ( 'NONE',  ( -9.749377714296398878, 10.28442384816749922, -229.3722863967025205 ) ) ;
#15165 = CARTESIAN_POINT ( 'NONE',  ( -12.37311134093142506, -6.729359123088276995, -218.5215259163429380 ) ) ;
#15166 = CARTESIAN_POINT ( 'NONE',  ( -27.49181041625929467, 3.366775762903781044E-15, 89.13175911166534604 ) ) ;
#15167 = CARTESIAN_POINT ( 'NONE',  ( 11.87982377808925527, 10.85265283465803421, -229.5027252913499183 ) ) ;
#15168 = CARTESIAN_POINT ( 'NONE',  ( -23.00000000000009237, 0.000000000000000000, -75.00000000000000000 ) ) ;
#15169 = CARTESIAN_POINT ( 'NONE',  ( 13.91151814069282722, -15.58123622716646572, -216.5183035683795367 ) ) ;
#15170 = CARTESIAN_POINT ( 'NONE',  ( -13.92046207272054303, -0.1600067567908077248, -224.5811699126800818 ) ) ;
#15171 = PRODUCT_DEFINITION_SHAPE ( 'NONE', 'NONE',  #22273 ) ;
#15172 = CARTESIAN_POINT ( 'NONE',  ( -13.48133478602219171, 10.24771958306113362, -218.3822527490931691 ) ) ;
#15173 = CARTESIAN_POINT ( 'NONE',  ( 27.58248235015124550, 10.80791576765187934, -226.6933256641281389 ) ) ;
#15174 = CARTESIAN_POINT ( 'NONE',  ( -5.688232406366994454, -14.80527619068227629, -228.6723097085491645 ) ) ;
#15175 = CIRCLE ( 'NONE', #14797, 3.000000000000002665 ) ;
#15176 = CARTESIAN_POINT ( 'NONE',  ( 13.54927135793711557, 0.6749664302445949060, -222.0769159577524192 ) ) ;
#15177 = CARTESIAN_POINT ( 'NONE',  ( 18.80535572547204382, -2.962702208451977626, -224.5130642812128485 ) ) ;
#15178 = CARTESIAN_POINT ( 'NONE',  ( 16.23205080756887853, 0.000000000000000000, 95.00000000000000000 ) ) ;
#15179 = CARTESIAN_POINT ( 'NONE',  ( 15.67226265972355392, -3.922905252720024105, -226.2579514984929858 ) ) ;
#15181 = EDGE_CURVE ( 'NONE', #8832, #9492, #12042, .T. ) ;
#15180 = CARTESIAN_POINT ( 'NONE',  ( 14.44181943480797159, -1.924641616899158914, -227.3019274429727830 ) ) ;
#15182 = DIRECTION ( 'NONE',  ( -1.000000000000000000, 0.000000000000000000, 0.000000000000000000 ) ) ;
#15183 = CIRCLE ( 'NONE', #15904, 19.63401512838747820 ) ;
#15184 = DIRECTION ( 'NONE',  ( 1.000000000000000000, 0.000000000000000000, 0.000000000000000000 ) ) ;
#15185 = CARTESIAN_POINT ( 'NONE',  ( 5.064106757301036765, 16.06517852189101703, -221.6413221086847329 ) ) ;
#15186 = CARTESIAN_POINT ( 'NONE',  ( 17.65733440236621732, -13.95165017647719452, -214.8231966952668301 ) ) ;
#15187 = CARTESIAN_POINT ( 'NONE',  ( 12.31511859722645852, -8.491226738247512174, -220.9006323875693738 ) ) ;
#15188 = EDGE_LOOP ( 'NONE', ( #11013, #20923 ) ) ;
#15189 = CARTESIAN_POINT ( 'NONE',  ( -9.627017372966443887, 15.60690227900018279, -218.8878023709062859 ) ) ;
#15190 = CARTESIAN_POINT ( 'NONE',  ( 24.19635128940818447, 10.31396593861802380, -216.9479509989864425 ) ) ;
#15191 = CARTESIAN_POINT ( 'NONE',  ( 21.68053922431529301, 13.05890675940072931, -230.5667798303363440 ) ) ;
#15192 = EDGE_LOOP ( 'NONE', ( #18491, #15557, #543, #19895 ) ) ;
#15193 = CARTESIAN_POINT ( 'NONE',  ( -2.652888268066178945, -28.18865072326549637, -221.4226523288203623 ) ) ;
#15194 = CARTESIAN_POINT ( 'NONE',  ( -9.211115167980509000, -5.709328484389684100, 92.00000000000001421 ) ) ;
#15195 = CARTESIAN_POINT ( 'NONE',  ( -9.924247690135956645, 7.079756654796299564, -222.1205998075789694 ) ) ;
#15196 = CARTESIAN_POINT ( 'NONE',  ( 12.56362091610784049, 9.747446748398973071, -231.6428467497164547 ) ) ;
#15197 = CARTESIAN_POINT ( 'NONE',  ( 9.379155480182538085, -13.23755613463586300, -225.9392943819708250 ) ) ;
#15198 = EDGE_CURVE ( 'NONE', #7178, #2436, #1355, .T. ) ;
#15199 = CARTESIAN_POINT ( 'NONE',  ( 5.141746912158045468, 22.01688500372448232, -216.6678693612369386 ) ) ;
#15200 = CARTESIAN_POINT ( 'NONE',  ( -22.47200958260654957, 4.697452857301940732, -216.5879371680706242 ) ) ;
#15201 = AXIS2_PLACEMENT_3D ( 'NONE', #17221, #15765, #9006 ) ;
#15202 = CARTESIAN_POINT ( 'NONE',  ( 24.61409543538958289, 19.88121288930873476, -228.5015986536257344 ) ) ;
#15203 = CARTESIAN_POINT ( 'NONE',  ( -14.08236938285573636, 6.062428076406559008, -221.7923619418395447 ) ) ;
#15204 = APPLICATION_CONTEXT ( 'automotive_design' ) ;
#15205 = CARTESIAN_POINT ( 'NONE',  ( -7.395406416482832590, 12.93623984139929739, -219.2606224730616873 ) ) ;
#15206 = CARTESIAN_POINT ( 'NONE',  ( 20.34032485158648029, 2.741617426884598530, -217.9827731991294968 ) ) ;
#15207 = CARTESIAN_POINT ( 'NONE',  ( 1.455106383990497187, 21.12056149333958999, -230.8076663600630241 ) ) ;
#15208 = PLANE ( 'NONE',  #88 ) ;
#15209 = DIRECTION ( 'NONE',  ( -1.000000000000000000, 0.000000000000000000, 0.000000000000000000 ) ) ;
#15210 = CARTESIAN_POINT ( 'NONE',  ( -20.85586116824185510, -1.996934699305910499, -232.3804859832740135 ) ) ;
#15211 = CARTESIAN_POINT ( 'NONE',  ( -12.13692969104051400, -0.3108940857385004697, -222.6170402347994184 ) ) ;
#15212 = CARTESIAN_POINT ( 'NONE',  ( -11.03528491614390994, -18.43141318057359612, -232.7233776306152038 ) ) ;
#15213 = AXIS2_PLACEMENT_3D ( 'NONE', #6687, #39, #10503 ) ;
#15214 = CARTESIAN_POINT ( 'NONE',  ( 21.65323058444409199, 0.3442074641359742504, -227.9814296144337220 ) ) ;
#15215 = VECTOR ( 'NONE', #2510, 1000.000000000000000 ) ;
#15216 = CARTESIAN_POINT ( 'NONE',  ( -13.51991436508781597, 16.61129329384914755, -232.1184346153593197 ) ) ;
#15217 = CARTESIAN_POINT ( 'NONE',  ( 4.788325992165110456, -24.70830725884669121, -218.5516572218182603 ) ) ;
#15218 = CARTESIAN_POINT ( 'NONE',  ( 24.20411255886326529, 12.66254860825103634, -218.0144359054998802 ) ) ;
#15219 = CARTESIAN_POINT ( 'NONE',  ( -4.866400999161825780, 25.69921167300892861, -231.0100031340613782 ) ) ;
#15220 = CARTESIAN_POINT ( 'NONE',  ( -10.49339404011726984, 12.66576824096800991, -217.2681947942554643 ) ) ;
#15221 = ORIENTED_EDGE ( 'NONE', *, *, #15873, .F. ) ;
#15222 = CARTESIAN_POINT ( 'NONE',  ( 28.41126862162173694, -7.739794849403359933, -232.1728475156252500 ) ) ;
#15223 = VERTEX_POINT ( 'NONE', #115 ) ;
#15224 = CARTESIAN_POINT ( 'NONE',  ( 12.10245006109274080, 26.02147364279441888, -220.6079829738538649 ) ) ;
#15225 = CARTESIAN_POINT ( 'NONE',  ( -17.59913672443795463, -0.5356773789333074687, -220.7342471185320960 ) ) ;
#15226 = CARTESIAN_POINT ( 'NONE',  ( -16.66929017373293931, 3.065794289431343689, -220.7800282905443794 ) ) ;
#15227 = CARTESIAN_POINT ( 'NONE',  ( 22.96914677622851642, 0.000000000000000000, 75.00000000000000000 ) ) ;
#15228 = CARTESIAN_POINT ( 'NONE',  ( -28.63642022368215478, -8.327690832987633129, -230.6787490302224057 ) ) ;
#15229 = CARTESIAN_POINT ( 'NONE',  ( 15.88043104796248528, 11.88135572392608807, -216.2525917828042168 ) ) ;
#15230 = CARTESIAN_POINT ( 'NONE',  ( -16.51501534778698854, 10.61825396983174485, -230.5082364903317966 ) ) ;
#15231 = VECTOR ( 'NONE', #19415, 1000.000000000000000 ) ;
#15232 = CARTESIAN_POINT ( 'NONE',  ( -6.260151855817680300, 29.88549235135308635, -226.8929519981915064 ) ) ;
#15233 = CARTESIAN_POINT ( 'NONE',  ( 15.07212457412616224, 2.472408313530222390, -227.3472192494155024 ) ) ;
#15234 = CARTESIAN_POINT ( 'NONE',  ( -8.876630286717240637, -14.53920553942005256, -232.5681369007955368 ) ) ;
#15235 = ORIENTED_EDGE ( 'NONE', *, *, #7732, .T. ) ;
#15236 = CARTESIAN_POINT ( 'NONE',  ( -10.46545893407769157, -9.768586176915025732, -226.8636372813723199 ) ) ;
#15237 = CARTESIAN_POINT ( 'NONE',  ( -23.68377094563794572, 13.02263794644603578, -215.9752901280847652 ) ) ;
#15238 = CARTESIAN_POINT ( 'NONE',  ( 2.378655016347637652, -14.31292064579845302, -219.9942319014987220 ) ) ;
#15239 = CARTESIAN_POINT ( 'NONE',  ( -0.3969026096611234511, 20.89748314411456676, -216.3289738411752978 ) ) ;
#15240 = CARTESIAN_POINT ( 'NONE',  ( 12.92161125358352791, -8.797851723037126703, -217.2061419145261425 ) ) ;
#15241 = CARTESIAN_POINT ( 'NONE',  ( -14.93108815068229589, -1.792787290847115633, -227.6165763581034582 ) ) ;
#15242 = CARTESIAN_POINT ( 'NONE',  ( 10.98110116949302828, 13.70618071521442971, -230.2797640191687378 ) ) ;
#15243 = DIRECTION ( 'NONE',  ( 1.224646799147353207E-16, 1.000000000000000000, 0.000000000000000000 ) ) ;
#15244 = CARTESIAN_POINT ( 'NONE',  ( -13.40354389326479456, 23.35336998323175450, -219.8517474526506987 ) ) ;
#15245 = CARTESIAN_POINT ( 'NONE',  ( 21.46274988498219471, 20.25395488059580984, -223.1777011585387243 ) ) ;
#15246 = CARTESIAN_POINT ( 'NONE',  ( 15.85665641241444668, 18.24713744004561988, -217.7195292979064902 ) ) ;
#15247 = CARTESIAN_POINT ( 'NONE',  ( 18.75523091462765990, 19.46592657336209697, -230.4909883316157391 ) ) ;
#15248 = CARTESIAN_POINT ( 'NONE',  ( -2.170317331930874172, -31.11073952835316803, -223.3804330553629995 ) ) ;
#15249 = CARTESIAN_POINT ( 'NONE',  ( -10.45265333418718612, 16.71118685480038479, -231.7490466715443631 ) ) ;
#15250 = EDGE_CURVE ( 'NONE', #12719, #14946, #11688, .T. ) ;
#15251 = CARTESIAN_POINT ( 'NONE',  ( -21.89482327431018760, 1.733733432562314158, -233.1353281693111796 ) ) ;
#15252 = FACE_OUTER_BOUND ( 'NONE', #9965, .T. ) ;
#15253 = CARTESIAN_POINT ( 'NONE',  ( 15.05360126642391450, 1.481754003466396963, -222.9454997252120734 ) ) ;
#15254 = CARTESIAN_POINT ( 'NONE',  ( 15.36293661829273027, -24.44941682316833464, -223.0188286856611626 ) ) ;
#15255 = CARTESIAN_POINT ( 'NONE',  ( -13.31590776630363315, 5.340120742929252096, -225.6956515496373186 ) ) ;
#15256 = CARTESIAN_POINT ( 'NONE',  ( 2.951582164238582440, 19.39026647431845873, -217.4356918981242472 ) ) ;
#15257 = CARTESIAN_POINT ( 'NONE',  ( -26.07210576407111446, -8.413030596423759278, -230.6002792590230115 ) ) ;
#15258 = CONTEXT_DEPENDENT_SHAPE_REPRESENTATION ( #21063, #13739 ) ;
#15259 = CARTESIAN_POINT ( 'NONE',  ( 14.00715608756928532, 4.299235856235253728, -230.2440235370780215 ) ) ;
#15260 = CARTESIAN_POINT ( 'NONE',  ( 10.35958063030883025, 8.003303894222913328, -225.9303204057916048 ) ) ;
#15261 = CARTESIAN_POINT ( 'NONE',  ( -3.060450601941519189, 13.29454208326677289, -222.0135664617158682 ) ) ;
#15262 = CARTESIAN_POINT ( 'NONE',  ( 26.05530571436537457, -9.878918321867194763, -229.2327836737675284 ) ) ;
#15263 = CARTESIAN_POINT ( 'NONE',  ( 16.07480884343054939, -7.767425703123992164, -217.5935768756353923 ) ) ;
#15264 = VECTOR ( 'NONE', #13452, 1000.000000000000000 ) ;
#15265 = CARTESIAN_POINT ( 'NONE',  ( -2.817219543927646175, 14.13981714106644993, -229.6779615865167443 ) ) ;
#15266 = CARTESIAN_POINT ( 'NONE',  ( -22.27532461284199528, -3.712691205162892416, -215.8122794664481603 ) ) ;
#15267 = CARTESIAN_POINT ( 'NONE',  ( -2.270280637033633475, -14.48864307936496765, -230.4581659391201072 ) ) ;
#15268 = CARTESIAN_POINT ( 'NONE',  ( 8.649266908999912573, -10.50942778440553482, -226.4415026780416440 ) ) ;
#15269 = CARTESIAN_POINT ( 'NONE',  ( -14.83806045519817829, 13.18806197935771074, -233.4179411789645542 ) ) ;
#15270 = CARTESIAN_POINT ( 'NONE',  ( 5.195682580001069084, 14.86321519495278665, -224.7851167466743334 ) ) ;
#15271 = CARTESIAN_POINT ( 'NONE',  ( -15.20262116893801974, 8.038155052917188570, -217.6767387945475036 ) ) ;
#15272 = CARTESIAN_POINT ( 'NONE',  ( -15.64716994811699813, 6.210654946517923491, -217.0002936794128345 ) ) ;
#15273 = CARTESIAN_POINT ( 'NONE',  ( -13.72210242120180901, -11.34614737046836908, -229.0742334187831659 ) ) ;
#15274 = ORIENTED_EDGE ( 'NONE', *, *, #16032, .T. ) ;
#15275 = CARTESIAN_POINT ( 'NONE',  ( -4.067324790461362305, 15.10342260507846746, -228.2464404076259257 ) ) ;
#15276 = EDGE_CURVE ( 'NONE', #17859, #8719, #3143, .T. ) ;
#15277 = CARTESIAN_POINT ( 'NONE',  ( 20.76808360334631232, 5.412616674732960931, -234.1222385626545304 ) ) ;
#15278 = CARTESIAN_POINT ( 'NONE',  ( 16.71363093372661979, 20.70203100498337179, -215.6856694095356488 ) ) ;
#15279 = CARTESIAN_POINT ( 'NONE',  ( 28.46281617689634302, -10.50803404096709137, -222.5507679334694728 ) ) ;
#15280 = CARTESIAN_POINT ( 'NONE',  ( 1.455845656607146809E-13, -21.63401512838747820, 77.51594804401857175 ) ) ;
#15281 = ORIENTED_EDGE ( 'NONE', *, *, #4728, .T. ) ;
#15282 = CARTESIAN_POINT ( 'NONE',  ( -2.958555384449997661, 13.07587799061801093, -222.7767538261418565 ) ) ;
#15283 = CARTESIAN_POINT ( 'NONE',  ( -26.69331514234889013, -17.84497232456928373, -223.5918739730229845 ) ) ;
#15284 = DIRECTION ( 'NONE',  ( 0.000000000000000000, 0.000000000000000000, 1.000000000000000000 ) ) ;
#15285 = AXIS2_PLACEMENT_3D ( 'NONE', #9055, #11484, #15922 ) ;
#15286 = CARTESIAN_POINT ( 'NONE',  ( 21.25094435758043332, 17.68230636442804027, -229.7964888993842010 ) ) ;
#15287 = DIRECTION ( 'NONE',  ( 0.2588190451025213501, -3.169619151431772337E-17, 0.9659258262890680902 ) ) ;
#15288 = CARTESIAN_POINT ( 'NONE',  ( 16.85953475301105442, -7.801609028127129086, -231.9437213283852941 ) ) ;
#15289 = CARTESIAN_POINT ( 'NONE',  ( -25.80904414196669450, 12.19501778665756220, -219.1732313092283846 ) ) ;
#15290 = CARTESIAN_POINT ( 'NONE',  ( 16.56146809408446430, -0.9616313295950813522, -228.5729530379900609 ) ) ;
#15291 = CARTESIAN_POINT ( 'NONE',  ( -11.96638064467250473, -24.81952708901905069, -229.8544473269683692 ) ) ;
#15292 = CARTESIAN_POINT ( 'NONE',  ( 0.000000000000000000, -17.50000000000000711, -24.99999999999999645 ) ) ;
#15293 = CARTESIAN_POINT ( 'NONE',  ( 18.89697753402895586, -2.884212079946346652, -224.1661613968960864 ) ) ;
#15294 = FACE_OUTER_BOUND ( 'NONE', #5320, .T. ) ;
#15295 = CARTESIAN_POINT ( 'NONE',  ( 12.89891433044458502, -16.86700836158627936, -231.6320225002741040 ) ) ;
#15296 = CARTESIAN_POINT ( 'NONE',  ( -22.05223281125446633, 0.4748437386657422543, -217.8785187290425256 ) ) ;
#15297 = CARTESIAN_POINT ( 'NONE',  ( 0.000000000000000000, 0.000000000000000000, -60.00000000000001421 ) ) ;
#15298 = CARTESIAN_POINT ( 'NONE',  ( 11.05872493453861161, 12.09300746323778775, -226.7727269015348952 ) ) ;
#15299 = CARTESIAN_POINT ( 'NONE',  ( 5.720314275582434327, 25.17872937134267630, -219.7530083620574430 ) ) ;
#15300 = CARTESIAN_POINT ( 'NONE',  ( 18.85502272441424765, -23.46047257272994102, -219.5236553823413317 ) ) ;
#15301 = CARTESIAN_POINT ( 'NONE',  ( 14.99336262864975211, -23.54026314425397004, -231.3018640253376361 ) ) ;
#15302 = ORIENTED_EDGE ( 'NONE', *, *, #15761, .T. ) ;
#15303 = CIRCLE ( 'NONE', #4866, 21.99162546567091070 ) ;
#15304 = EDGE_CURVE ( 'NONE', #22262, #12810, #10026, .T. ) ;
#15305 = CARTESIAN_POINT ( 'NONE',  ( -7.375127652145912371, 13.01042140126078195, -223.9959097520547004 ) ) ;
#15306 = CARTESIAN_POINT ( 'NONE',  ( -27.28038240442402440, 5.683827137705129040, -226.0726697751923382 ) ) ;
#15307 = CARTESIAN_POINT ( 'NONE',  ( 14.68130101653174613, 6.427210486143660084, -228.0153742661088074 ) ) ;
#15308 = VERTEX_POINT ( 'NONE', #17220 ) ;
#15309 = CARTESIAN_POINT ( 'NONE',  ( -7.103355004864593703, -14.30675315766165312, -225.9889059232917532 ) ) ;
#15310 = DIRECTION ( 'NONE',  ( -1.000000000000000000, 0.000000000000000000, 0.000000000000000000 ) ) ;
#15311 = ORIENTED_EDGE ( 'NONE', *, *, #16633, .T. ) ;
#15312 = ORIENTED_EDGE ( 'NONE', *, *, #16421, .T. ) ;
#15313 = CARTESIAN_POINT ( 'NONE',  ( 6.839751633953758514, 19.11639828585652623, -235.1218211620789873 ) ) ;
#15314 = CARTESIAN_POINT ( 'NONE',  ( 11.86025528723659050, -11.55469215893994850, -227.5711990284272872 ) ) ;
#15315 = CARTESIAN_POINT ( 'NONE',  ( 10.66614775643814994, 26.29080367171353672, -230.0818785118670178 ) ) ;
#15316 = CARTESIAN_POINT ( 'NONE',  ( -13.92046207272054303, -0.1600067567908077248, -224.5811699126800818 ) ) ;
#15317 = ADVANCED_FACE ( 'NONE', ( #1463 ), #9891, .T. ) ;
#15318 = CARTESIAN_POINT ( 'NONE',  ( 21.77779027533950540, 18.43917590911969029, -232.9503911151153659 ) ) ;
#15319 = PRESENTATION_LAYER_ASSIGNMENT (  '', '', ( #21759 ) ) ;
#15320 = CARTESIAN_POINT ( 'NONE',  ( -19.35155980425159683, 1.157993580480985552, -230.3698774940947942 ) ) ;
#15321 = CARTESIAN_POINT ( 'NONE',  ( -17.17400284685640344, 24.63223427531467280, -220.6313524368512162 ) ) ;
#15322 = CYLINDRICAL_SURFACE ( 'NONE', #1925, 3.000000000000002665 ) ;
#15323 = CARTESIAN_POINT ( 'NONE',  ( 5.434900225474387447, -11.93567727083262042, -224.7511004068755369 ) ) ;
#15324 = CARTESIAN_POINT ( 'NONE',  ( 19.63495056682994289, -4.096126682090319271, -232.1271738766904207 ) ) ;
#15325 = LINE ( 'NONE', #13514, #21725 ) ;
#15326 = CARTESIAN_POINT ( 'NONE',  ( -23.10791503177032880, -5.282985115830100220, -217.6364121950018671 ) ) ;
#15327 = CARTESIAN_POINT ( 'NONE',  ( -11.89542918462869103, -0.2773029175206048191, -224.4556830488584467 ) ) ;
#15328 = CARTESIAN_POINT ( 'NONE',  ( -23.54933555373352050, -14.29320362656835997, -227.5895276738501423 ) ) ;
#15329 = CARTESIAN_POINT ( 'NONE',  ( 19.08116649778970952, 2.725278401796274341, -226.2588043811726379 ) ) ;
#15330 = CARTESIAN_POINT ( 'NONE',  ( 4.725966861008204845, -14.24791254766627624, -227.2781441550517343 ) ) ;
#15331 = CARTESIAN_POINT ( 'NONE',  ( -14.07336028695978314, 1.752429266630609828, -222.9750305084206161 ) ) ;
#15332 = CARTESIAN_POINT ( 'NONE',  ( -7.240690404266621805, 13.01623002570985044, -225.3000933658701967 ) ) ;
#15333 = CARTESIAN_POINT ( 'NONE',  ( -6.079211283031130897, 16.94466709905296753, -232.9163774423793711 ) ) ;
#15334 = ORIENTED_EDGE ( 'NONE', *, *, #15829, .T. ) ;
#15335 = CARTESIAN_POINT ( 'NONE',  ( 15.86371404000427887, -2.776058937659206638, -233.1947532464443213 ) ) ;
#15336 = CARTESIAN_POINT ( 'NONE',  ( 8.496844655769807630, 14.66037471857024599, -219.1631158796573118 ) ) ;
#15337 = COLOUR_RGB ( '', 0.31764706, 0.68627451, 0.89019608) ;
#15338 = CARTESIAN_POINT ( 'NONE',  ( -18.88344489807484905, 1.071113352238720617, -230.0966926586188208 ) ) ;
#15339 = CARTESIAN_POINT ( 'NONE',  ( -18.04102731735134313, 0.8647102676311391178, -229.4625228093430849 ) ) ;
#15340 = CARTESIAN_POINT ( 'NONE',  ( 16.55626903245587656, 22.80423546114836952, -218.9884947126587633 ) ) ;
#15341 = CARTESIAN_POINT ( 'NONE',  ( -15.83894155097017631, 1.950284868793920712, -224.5615909987450038 ) ) ;
#15342 = CARTESIAN_POINT ( 'NONE',  ( 1.660345614755502686, 12.19060476922103931, -223.1112690039082906 ) ) ;
#15343 = CARTESIAN_POINT ( 'NONE',  ( 16.31458447723494132, 2.619382102851042671, -229.5862799001085364 ) ) ;
#15344 = CARTESIAN_POINT ( 'NONE',  ( -20.46754208161335598, -23.96478097336112256, -223.3311283152840758 ) ) ;
#15345 = ORIENTED_EDGE ( 'NONE', *, *, #16713, .F. ) ;
#15346 = CARTESIAN_POINT ( 'NONE',  ( -12.79488508867961549, -11.10380203712096581, -230.9440799972209106 ) ) ;
#15347 = ADVANCED_FACE ( 'NONE', ( #13738 ), #22055, .F. ) ;
#15348 = CARTESIAN_POINT ( 'NONE',  ( -9.045741320599788082, 11.46901338045063312, -219.0588111342715365 ) ) ;
#15349 = CARTESIAN_POINT ( 'NONE',  ( 1.836136847161299990, -12.84546502099244591, -226.1727064218434293 ) ) ;
#15350 = CARTESIAN_POINT ( 'NONE',  ( -3.855805549595750392, 26.68244055262801950, -232.4569730455296508 ) ) ;
#15351 = CARTESIAN_POINT ( 'NONE',  ( 27.04962740251871978, -7.854494666110665158, -217.8595067830158882 ) ) ;
#15352 = CARTESIAN_POINT ( 'NONE',  ( -28.18501077041064562, -8.523171531337160545, -227.0531053546762337 ) ) ;
#15353 = ADVANCED_FACE ( 'NONE', ( #6644 ), #18904, .F. ) ;
#15354 = CARTESIAN_POINT ( 'NONE',  ( 11.54460987479198053, 9.649171130674412566, -228.7280371210653698 ) ) ;
#15355 = DIRECTION ( 'NONE',  ( -1.000000000000000000, 0.000000000000000000, 0.000000000000000000 ) ) ;
#15356 = CARTESIAN_POINT ( 'NONE',  ( -8.463283775975803280, 12.69606588598396613, -228.6351674091961286 ) ) ;
#15357 = CARTESIAN_POINT ( 'NONE',  ( 26.51393280883522863, 15.12455065102723495, -226.1955201378414415 ) ) ;
#15358 = CARTESIAN_POINT ( 'NONE',  ( 14.68783945462866924, 9.535285537539673228, -219.4694094309942045 ) ) ;
#15359 = CARTESIAN_POINT ( 'NONE',  ( 8.829458998963966465, 22.90677303676718779, -219.2026791561175685 ) ) ;
#15360 = CARTESIAN_POINT ( 'NONE',  ( 3.784839621866231241, -12.46827349529254469, -229.8854786719440426 ) ) ;
#15361 = CARTESIAN_POINT ( 'NONE',  ( -2.121548062149551495, 13.26065194155116345, -221.8830439064491884 ) ) ;
#15362 = PRODUCT_DEFINITION_SHAPE ( 'NONE', 'NONE',  #6428 ) ;
#15363 = CARTESIAN_POINT ( 'NONE',  ( 28.02123297569005089, 5.903198806000402143, -227.5759114383273811 ) ) ;
#15364 = CARTESIAN_POINT ( 'NONE',  ( 9.745394341301471641, -28.41975495766811832, -225.7559345954832963 ) ) ;
#15365 = CARTESIAN_POINT ( 'NONE',  ( -15.11329978779464689, 11.41628732213579411, -231.7124318929555500 ) ) ;
#15366 = CARTESIAN_POINT ( 'NONE',  ( 2.508382434586714282, 15.09451298870656011, -220.9010239894319625 ) ) ;
#15367 = CARTESIAN_POINT ( 'NONE',  ( -16.75313578746775889, -14.38352658620038937, -216.6304878158699978 ) ) ;
#15368 = CARTESIAN_POINT ( 'NONE',  ( 17.22423229049764970, 1.395540479540137380, -217.3898520248025363 ) ) ;
#15369 = CARTESIAN_POINT ( 'NONE',  ( 12.46318849118074112, 25.01309605388695445, -216.9820503660967859 ) ) ;
#15370 = ORIENTED_EDGE ( 'NONE', *, *, #1716, .F. ) ;
#15371 = CARTESIAN_POINT ( 'NONE',  ( 7.769483725421269860, 20.68783433326350263, -233.2348178266662728 ) ) ;
#15372 = CARTESIAN_POINT ( 'NONE',  ( 15.03150297321239925, -8.313127316319620874, -220.7815108570360394 ) ) ;
#15373 = CARTESIAN_POINT ( 'NONE',  ( 23.17317677245511831, -6.950782331930943414, -233.5406539459643227 ) ) ;
#15374 = CARTESIAN_POINT ( 'NONE',  ( 0.000000000000000000, 0.000000000000000000, -75.00000000000000000 ) ) ;
#15375 = CARTESIAN_POINT ( 'NONE',  ( 0.4042326456706432647, 15.50845657815858303, -219.2680337625893401 ) ) ;
#15376 = CARTESIAN_POINT ( 'NONE',  ( -15.15102066082706678, -13.26725641419114510, -214.8414790003043322 ) ) ;
#15377 = CARTESIAN_POINT ( 'NONE',  ( -6.512931564893298386, -17.32529878264574563, -216.7284160531958719 ) ) ;
#15378 = CARTESIAN_POINT ( 'NONE',  ( 6.374306683232226156, -13.38367253400339330, -219.9651431149896723 ) ) ;
#15379 = CARTESIAN_POINT ( 'NONE',  ( -18.16160515720599022, 12.42447964075808997, -216.1086293678848449 ) ) ;
#15380 = CARTESIAN_POINT ( 'NONE',  ( 15.70200226922815290, 22.14006925444000018, -227.8255507828836244 ) ) ;
#15381 = CARTESIAN_POINT ( 'NONE',  ( -12.78558550453068854, 7.693178343823584342, -230.0800953344970878 ) ) ;
#15382 = CARTESIAN_POINT ( 'NONE',  ( -30.35034897870229287, 7.696526532841741819, -221.5749790623549416 ) ) ;
#15383 = CARTESIAN_POINT ( 'NONE',  ( -22.54540532658949914, -16.00113133426942724, -227.3151344909721843 ) ) ;
#15384 = VERTEX_POINT ( 'NONE', #22171 ) ;
#15385 = CARTESIAN_POINT ( 'NONE',  ( -10.91003322996498071, 12.84665145358222382, -229.9786893781767958 ) ) ;
#15386 = CARTESIAN_POINT ( 'NONE',  ( 24.81079154715000357, 3.171651085595392772, -216.4177249688571578 ) ) ;
#15387 = CARTESIAN_POINT ( 'NONE',  ( 11.31331191788792623, 29.23420701778062281, -220.7538464529627333 ) ) ;
#15388 = CARTESIAN_POINT ( 'NONE',  ( 10.73531068932428667, -10.59494929936097307, -229.0901643129046192 ) ) ;
#15389 = CYLINDRICAL_SURFACE ( 'NONE', #16487, 2.000000000000000000 ) ;
#15390 = EDGE_LOOP ( 'NONE', ( #1514, #7272, #6137, #13763 ) ) ;
#15391 = CARTESIAN_POINT ( 'NONE',  ( -8.501641725227710111, 25.47064987787527102, -217.3358698761548737 ) ) ;
#15392 = CARTESIAN_POINT ( 'NONE',  ( -18.30187879049682209, -3.992092017665997972, -215.1717549395094693 ) ) ;
#15393 = CARTESIAN_POINT ( 'NONE',  ( 26.00000000000000000, -3.600000000000001421, -2.699999999999999289 ) ) ;
#15394 = CARTESIAN_POINT ( 'NONE',  ( 28.57344184061583192, 5.631897254180425527, -225.1192013637692355 ) ) ;
#15395 = CARTESIAN_POINT ( 'NONE',  ( -26.02440924314744919, 2.824604386891162111, -232.0644005296583430 ) ) ;
#15396 = CARTESIAN_POINT ( 'NONE',  ( 9.918856707546316542, -11.48950767347732871, -219.9734948840342668 ) ) ;
#15397 = SURFACE_SIDE_STYLE ('',( #20540 ) ) ;
#15398 = CARTESIAN_POINT ( 'NONE',  ( -14.29986196492902550, 0.06805469746732484282, -227.4167624117703213 ) ) ;
#15399 = CARTESIAN_POINT ( 'NONE',  ( 15.28706223449149348, 2.473424253736659306, -227.9634568993954531 ) ) ;
#15400 = CARTESIAN_POINT ( 'NONE',  ( -1.339836966046043631, -21.49735173129188581, -217.9043760890963313 ) ) ;
#15401 = CARTESIAN_POINT ( 'NONE',  ( 1.322875655532295358, 1.500000000000000000, -104.9999999999999858 ) ) ;
#15402 = CARTESIAN_POINT ( 'NONE',  ( 14.85123888640019452, 5.067529763532427012, -221.9058491819374979 ) ) ;
#15403 = CARTESIAN_POINT ( 'NONE',  ( -17.84981083811007707, 0.8485253248287054628, -231.8041300026935119 ) ) ;
#15404 = CARTESIAN_POINT ( 'NONE',  ( 22.59847068942421444, -14.29990159211854106, -221.3422834976353499 ) ) ;
#15405 = CARTESIAN_POINT ( 'NONE',  ( 12.79806454121929349, -2.903405038957567186, -225.7792874317651410 ) ) ;
#15406 = CARTESIAN_POINT ( 'NONE',  ( -23.00000000000000000, 0.000000000000000000, 69.99999999999998579 ) ) ;
#15407 = CARTESIAN_POINT ( 'NONE',  ( 5.195682580001069084, 14.86321519495278665, -224.7851167466743334 ) ) ;
#15408 = CIRCLE ( 'NONE', #8582, 23.00000000000000000 ) ;
#15409 = CARTESIAN_POINT ( 'NONE',  ( 9.280831573919673616, 14.67893982993557422, -228.6940810986570796 ) ) ;
#15410 = CARTESIAN_POINT ( 'NONE',  ( 15.43596206743521826, -16.12492210025319750, -235.0559386399467314 ) ) ;
#15411 = CARTESIAN_POINT ( 'NONE',  ( 7.958080982411646076, -16.12895853103474408, -217.0903302464454612 ) ) ;
#15412 = ORIENTED_EDGE ( 'NONE', *, *, #7888, .F. ) ;
#15413 = CARTESIAN_POINT ( 'NONE',  ( -16.74094048923576494, 16.03040267675914521, -217.9177456399057178 ) ) ;
#15414 = CARTESIAN_POINT ( 'NONE',  ( -14.67397018911906770, 9.031553917454052893, -228.4349422195089119 ) ) ;
#15415 = CARTESIAN_POINT ( 'NONE',  ( 15.08139719848974103, 12.15862464477973504, -219.3112749338812080 ) ) ;
#15416 = ORIENTED_EDGE ( 'NONE', *, *, #6454, .T. ) ;
#15417 = CARTESIAN_POINT ( 'NONE',  ( -7.149118023545313783, -16.86598457999096823, -220.1902049135764514 ) ) ;
#15418 = CARTESIAN_POINT ( 'NONE',  ( -14.50024104873820185, 0.1235481402557507408, 93.00000000000000000 ) ) ;
#15419 = ORIENTED_EDGE ( 'NONE', *, *, #19438, .F. ) ;
#15420 = CARTESIAN_POINT ( 'NONE',  ( 15.07212457412616224, 2.472408313530222390, -227.3472192494155024 ) ) ;
#15421 = CARTESIAN_POINT ( 'NONE',  ( 13.12950778469841318, -23.99547238938880511, -222.5250877844293029 ) ) ;
#15422 = CARTESIAN_POINT ( 'NONE',  ( 6.093530912645064745, 16.79941505724243811, -232.1766444656230419 ) ) ;
#15423 = CARTESIAN_POINT ( 'NONE',  ( -9.151299407007059017, 9.196974979111923076, -223.9483834032048719 ) ) ;
#15424 = VECTOR ( 'NONE', #9542, 1000.000000000000000 ) ;
#15425 = CARTESIAN_POINT ( 'NONE',  ( 13.49694890958685711, 2.186465430673721677, -228.8273158381700512 ) ) ;
#15426 = CARTESIAN_POINT ( 'NONE',  ( -18.47334320050258327, 24.79293862780133040, -226.9986786077537317 ) ) ;
#15427 = CARTESIAN_POINT ( 'NONE',  ( 1.259348629394230867, 10.71767081544559552, 92.00000000000001421 ) ) ;
#15428 = CARTESIAN_POINT ( 'NONE',  ( -0.8413160509385254615, -28.71376977722865931, -218.8117683208458288 ) ) ;
#15429 = CARTESIAN_POINT ( 'NONE',  ( 23.48720700658024896, -2.145453947144424500, -217.8824464111000054 ) ) ;
#15430 = DIRECTION ( 'NONE',  ( -6.982962677686266711E-15, 1.000000000000000000, 0.000000000000000000 ) ) ;
#15431 = CARTESIAN_POINT ( 'NONE',  ( -28.30937415889876618, -7.921132361018833556, -222.9755670691803857 ) ) ;
#15432 = CARTESIAN_POINT ( 'NONE',  ( 21.31262902390056624, 0.4111834581965390645, -232.0572713672585792 ) ) ;
#15433 = CARTESIAN_POINT ( 'NONE',  ( -24.13163560393529394, -13.84165259829251227, -223.2936513752361805 ) ) ;
#15434 =( NAMED_UNIT ( * ) PLANE_ANGLE_UNIT ( ) SI_UNIT ( $, .RADIAN. ) );
#15435 = CARTESIAN_POINT ( 'NONE',  ( 6.203932113039332563, -21.09630782756332223, -232.3325312104709894 ) ) ;
#15436 = CARTESIAN_POINT ( 'NONE',  ( -29.16153046926437753, 6.356672163541281506, -226.4393515956758165 ) ) ;
#15437 = CARTESIAN_POINT ( 'NONE',  ( 2.703362520412529779, 29.60004130108520215, -225.6165589735000481 ) ) ;
#15438 = CARTESIAN_POINT ( 'NONE',  ( -15.64710113362562183, 25.90300453978063189, -220.8637308366217269 ) ) ;
#15439 = EDGE_LOOP ( 'NONE', ( #20850, #8322, #3660, #3211, #15047 ) ) ;
#15440 = CARTESIAN_POINT ( 'NONE',  ( -22.11234321210701737, -3.359691084028018526, -230.9311713419302521 ) ) ;
#15441 = VERTEX_POINT ( 'NONE', #20465 ) ;
#15442 = CARTESIAN_POINT ( 'NONE',  ( 10.83706092800007781, 10.12544885278926543, -227.1716144446442343 ) ) ;
#15443 = CARTESIAN_POINT ( 'NONE',  ( -16.28135616697389310, 20.98764039357472200, -216.9434553755565958 ) ) ;
#15444 = CARTESIAN_POINT ( 'NONE',  ( -25.11055959288653128, 8.701823109978603199, -230.2231080656787583 ) ) ;
#15445 = CARTESIAN_POINT ( 'NONE',  ( -10.22552941266963877, -9.699191453761107695, -225.4315674810442545 ) ) ;
#15446 = CARTESIAN_POINT ( 'NONE',  ( -20.99999999999999645, 0.000000000000000000, -69.99999999999998579 ) ) ;
#15447 = CARTESIAN_POINT ( 'NONE',  ( 24.19635128940818447, 10.31396593861802380, -216.9479509989864425 ) ) ;
#15448 = CARTESIAN_POINT ( 'NONE',  ( -18.94009481283715957, 3.115208415279245191, -230.3622730452590588 ) ) ;
#15449 = CARTESIAN_POINT ( 'NONE',  ( 12.75306435971521068, 14.56583715532477186, -214.9711136650476533 ) ) ;
#15450 = CARTESIAN_POINT ( 'NONE',  ( 24.78377098693636427, 3.871650763546384155, -231.3521132786341923 ) ) ;
#15451 = CARTESIAN_POINT ( 'NONE',  ( -18.76818401764774080, -23.60322278862490109, -229.9112526505913365 ) ) ;
#15452 = CARTESIAN_POINT ( 'NONE',  ( -10.71823000853037655, -10.52987076429259794, -221.3501620068516331 ) ) ;
#15453 = CARTESIAN_POINT ( 'NONE',  ( -14.08083899843152231, 10.81596681319144970, -234.3239311387574446 ) ) ;
#15454 = CARTESIAN_POINT ( 'NONE',  ( 1.623338700557370951, -21.82196275546919040, -234.1129525514646730 ) ) ;
#15455 = CARTESIAN_POINT ( 'NONE',  ( -1.881996891245037995, 28.05344686410985489, -218.6379207300106202 ) ) ;
#15456 = CARTESIAN_POINT ( 'NONE',  ( 14.59690920037431638, -12.12875852167710988, -234.7370354398910877 ) ) ;
#15457 = CARTESIAN_POINT ( 'NONE',  ( -16.05483997570105714, -7.226811045751038165, -218.5819178105544438 ) ) ;
#15458 = EDGE_CURVE ( 'NONE', #21471, #15704, #13852, .T. ) ;
#15459 = CARTESIAN_POINT ( 'NONE',  ( -14.06164063153489252, 2.050767714179807744, -227.2881998904968270 ) ) ;
#15460 = CARTESIAN_POINT ( 'NONE',  ( -5.600903697806950632, 21.62055466701630735, -218.6671277943675307 ) ) ;
#15461 = CARTESIAN_POINT ( 'NONE',  ( 24.52160379727246209, 5.049198597839295033, -215.7868787176665535 ) ) ;
#15462 = CARTESIAN_POINT ( 'NONE',  ( 18.50911814746675788, 15.92944434255054453, -232.0449215596906072 ) ) ;
#15463 = CARTESIAN_POINT ( 'NONE',  ( 22.16327814861754675, 7.634676377199016706, -234.0520676664821735 ) ) ;
#15464 = CARTESIAN_POINT ( 'NONE',  ( 6.415926650623908323, -16.27382107952271895, -215.7995092914603674 ) ) ;
#15465 = CARTESIAN_POINT ( 'NONE',  ( 2.165130313308041288, 31.55305250914585002, -225.6791154433767304 ) ) ;
#15466 = CARTESIAN_POINT ( 'NONE',  ( 7.813662449283098610, -13.08401493520405445, -221.9442578939891177 ) ) ;
#15467 = CARTESIAN_POINT ( 'NONE',  ( -12.06153928353927540, 8.661506524875534296, -226.8425068572842349 ) ) ;
#15468 = EDGE_CURVE ( 'NONE', #9897, #20674, #14945, .T. ) ;
#15469 = CARTESIAN_POINT ( 'NONE',  ( 0.3632086708616291126, 21.06287758167331958, -232.5112839711303820 ) ) ;
#15470 = CARTESIAN_POINT ( 'NONE',  ( -15.74157322273402748, -13.22745315869835636, -216.7831660370879661 ) ) ;
#15471 = CARTESIAN_POINT ( 'NONE',  ( 22.42925200799500729, 5.652256920629083581, -234.0734181799116698 ) ) ;
#15472 = CARTESIAN_POINT ( 'NONE',  ( 17.10545320562996352, 22.53742678899184781, -232.4605876935045785 ) ) ;
#15473 = ORIENTED_EDGE ( 'NONE', *, *, #5375, .F. ) ;
#15474 = CARTESIAN_POINT ( 'NONE',  ( 11.13678936984666912, 26.95732789089726111, -228.8350761760834757 ) ) ;
#15475 = CARTESIAN_POINT ( 'NONE',  ( 14.12786214016513675, -4.771276416369937046, -223.8547069812204029 ) ) ;
#15476 = CARTESIAN_POINT ( 'NONE',  ( 21.85730963248023428, -9.423385237436111339, -216.6089804361807580 ) ) ;
#15477 = CARTESIAN_POINT ( 'NONE',  ( 20.41153371889344825, 17.18812948447019551, -230.7531656956970778 ) ) ;
#15478 = CARTESIAN_POINT ( 'NONE',  ( -19.82723516873631908, -6.367811336401608457, -234.7370909334860869 ) ) ;
#15479 = CARTESIAN_POINT ( 'NONE',  ( -6.012234575298915473, -13.00555924700598709, -229.4955436083688483 ) ) ;
#15480 = B_SPLINE_CURVE_WITH_KNOTS ( 'NONE', 3,
 ( #8977, #20998, #15841, #12468, #3892, #17636, #4436, #9526, #18406, #18297, #4771, #16602, #21766, #4660, #18188, #9410, #1071, #20073, #14704, #11647, #13119, #2856, #19744, #2968, #4324, #16719, #9740, #21652, #14598, #13335, #18519, #7838, #8170, #19849, #15036, #16385, #850, #7945, #14927, #19965, #16274, #7727, #1296, #964, #11533, #11428, #6466, #14809 ),
 .UNSPECIFIED., .F., .F.,
 ( 4, 2, 2, 2, 2, 2, 2, 2, 2, 2, 2, 2, 2, 2, 2, 2, 2, 2, 2, 2, 2, 2, 2, 4 ),
 ( 6.413919134271389359E-20, 0.001974931581232642393, 0.002962397371848964241, 0.003949863162465286522, 0.005924794743697927614, 0.006912260534314250762, 0.007899726324930574778, 0.009874657906163219340, 0.01184958948739586564, 0.01283705527801219139, 0.01382452106862851540, 0.01579945264986116343, 0.01678691844047748571, 0.01777438423109381493, 0.01974931581232645950, 0.02172424739355911100, 0.02271171318417543675, 0.02369917897479175903, 0.02567411055602440706, 0.02666157634664072934, 0.02764904213725705509, 0.02962397371848970312, 0.03061143950910603234, 0.03159890529972235462 ),
 .UNSPECIFIED. ) ;
#15481 = CARTESIAN_POINT ( 'NONE',  ( 5.451525948382545117, -12.45300865616632713, -227.8545162512558306 ) ) ;
#15482 = CARTESIAN_POINT ( 'NONE',  ( -3.130917144532865848, 26.01013079854885390, -229.4331404728494874 ) ) ;
#15483 = CARTESIAN_POINT ( 'NONE',  ( 21.68053922431529301, 13.05890675940072931, -230.5667798303363440 ) ) ;
#15484 = CARTESIAN_POINT ( 'NONE',  ( -13.58874046263339608, 12.73011668665171392, -216.5659449791897941 ) ) ;
#15485 = CARTESIAN_POINT ( 'NONE',  ( -10.30040261405712698, 19.75576125044891285, -218.0811964201226658 ) ) ;
#15486 = CARTESIAN_POINT ( 'NONE',  ( 16.07480884343054939, -7.767425703123992164, -217.5935768756353923 ) ) ;
#15487 = CARTESIAN_POINT ( 'NONE',  ( -7.240690404266621805, 13.01623002570985044, -225.3000933658701967 ) ) ;
#15488 = CARTESIAN_POINT ( 'NONE',  ( 25.62718606866737403, 13.33219119508369310, -230.9315691959737933 ) ) ;
#15489 = CARTESIAN_POINT ( 'NONE',  ( 25.41781277602550304, 19.49958712797920057, -223.1230538376805441 ) ) ;
#15490 = CARTESIAN_POINT ( 'NONE',  ( 16.26147397530412420, -13.20473954510486081, -216.9283256773164794 ) ) ;
#15491 = CARTESIAN_POINT ( 'NONE',  ( 14.46993441875745390, 0.2699826811589002284, -230.0986938382904157 ) ) ;
#15492 = ORIENTED_EDGE ( 'NONE', *, *, #7094, .T. ) ;
#15493 = CARTESIAN_POINT ( 'NONE',  ( 0.7245137624042983227, 13.44764381486384330, -223.4043886706536455 ) ) ;
#15494 = CARTESIAN_POINT ( 'NONE',  ( -27.51824122704870135, -10.15715933399136617, -232.3556155038515669 ) ) ;
#15495 = DIRECTION ( 'NONE',  ( -0.000000000000000000, -0.000000000000000000, -1.000000000000000000 ) ) ;
#15496 = CARTESIAN_POINT ( 'NONE',  ( 17.00168025137501004, 6.212099629982537508, -219.0548246536471595 ) ) ;
#15497 = CARTESIAN_POINT ( 'NONE',  ( 2.465190328815661892E-29, 24.63401512838760610, 77.51594804401857175 ) ) ;
#15498 = CARTESIAN_POINT ( 'NONE',  ( 17.15627899979664051, -18.64955541608202694, -217.1729447097152388 ) ) ;
#15499 = B_SPLINE_CURVE_WITH_KNOTS ( 'NONE', 3,
 ( #2208, #1879, #3566, #8762, #17197, #1773, #8647, #2102, #6959, #12131, #316, #15622, #15846, #15738, #5474, #13831, #20667, #7185, #17303, #18986, #17423, #10443, #7296, #203, #13942, #12241, #19092, #1992, #10671, #4349, #11455, #11679, #4687, #19770, #21567, #1214, #11561, #4803, #9997, #18104, #3117, #8089, #4467, #13147, #13034, #19880, #14956, #1098, #6156, #15066, #21796, #1435 ),
 .UNSPECIFIED., .F., .F.,
 ( 4, 2, 2, 2, 2, 2, 2, 2, 2, 2, 2, 2, 2, 2, 2, 2, 2, 2, 2, 2, 2, 2, 2, 2, 2, 4 ),
 ( 0.03159890529972235462, 0.03258572303769623896, 0.03357254077567013023, 0.03554617625161789890, 0.03653299398959179017, 0.03751981172756567451, 0.03949344720351345706, 0.04146708267946123266, 0.04245390041743511700, 0.04344071815540900827, 0.04541435363135679082, 0.04640117136933068209, 0.04738798910730457337, 0.04936162458325235591, 0.05034844232122625413, 0.05133526005920014540, 0.05232207779717404361, 0.05330889553514793489, 0.05528253101109571743, 0.05626934874906960871, 0.05725616648704350692, 0.05922980196299128253, 0.06021661970096517380, 0.06120343743893906507, 0.06219025517691295635, 0.06317707291488684762 ),
 .UNSPECIFIED. ) ;
#15500 = CARTESIAN_POINT ( 'NONE',  ( -13.93333636822611155, 3.327141996558931947, -221.4468162587888287 ) ) ;
#15501 = CARTESIAN_POINT ( 'NONE',  ( -14.07917727715460821, 7.534853284453274291, -218.6337090155677458 ) ) ;
#15502 = CARTESIAN_POINT ( 'NONE',  ( -4.994543945659216000, -15.01629888130124435, -221.3392717856295633 ) ) ;
#15503 = DIRECTION ( 'NONE',  ( -0.000000000000000000, -0.000000000000000000, 1.000000000000000000 ) ) ;
#15504 = CARTESIAN_POINT ( 'NONE',  ( -21.37887586799824646, 8.484154883082068110, 5.303148973211635031 ) ) ;
#15505 = CARTESIAN_POINT ( 'NONE',  ( -28.99926036811508467, 3.909990568804979194, -228.9613767892386988 ) ) ;
#15506 = CARTESIAN_POINT ( 'NONE',  ( 23.95414175253014477, -14.38191447464009087, -225.3623377062671125 ) ) ;
#15507 = CARTESIAN_POINT ( 'NONE',  ( 13.43601330613756595, -1.788726811927666915, -222.5908311466273517 ) ) ;
#15508 = CARTESIAN_POINT ( 'NONE',  ( 19.38023697009515800, -2.464236985537147095, -226.7227031297641986 ) ) ;
#15509 = CARTESIAN_POINT ( 'NONE',  ( 11.00580183749007190, 25.74996642444834904, -225.8602305833924788 ) ) ;
#15510 = CARTESIAN_POINT ( 'NONE',  ( 20.22510869507564024, 17.05975164568011238, -220.7829296213589316 ) ) ;
#15511 = CARTESIAN_POINT ( 'NONE',  ( 2.920206608988989760, -13.21961856575012639, -224.5557534934820865 ) ) ;
#15512 = CARTESIAN_POINT ( 'NONE',  ( 21.30961698559626427, -20.48616475849644303, -228.5322376518520002 ) ) ;
#15513 = ORIENTED_EDGE ( 'NONE', *, *, #6671, .T. ) ;
#15514 = CARTESIAN_POINT ( 'NONE',  ( -10.02095171162140019, 11.02119725306997111, -224.1251327387667516 ) ) ;
#15515 = CARTESIAN_POINT ( 'NONE',  ( -15.82068653568960137, 8.372322471091806051, -220.7139663195713979 ) ) ;
#15516 = CARTESIAN_POINT ( 'NONE',  ( -13.33011381921379090, 5.829915729572584304, -219.4453182727427816 ) ) ;
#15517 = CARTESIAN_POINT ( 'NONE',  ( -7.469054245001129466, -18.21857363335801594, -219.2823717272210047 ) ) ;
#15518 = CARTESIAN_POINT ( 'NONE',  ( -0.3188271712753658615, -10.76635261883074435, 92.00000000000002842 ) ) ;
#15519 = ORIENTED_EDGE ( 'NONE', *, *, #8330, .T. ) ;
#15520 = CARTESIAN_POINT ( 'NONE',  ( 24.60354977307301283, 7.993510024274534942, -218.5358880819990759 ) ) ;
#15521 = CARTESIAN_POINT ( 'NONE',  ( 8.587407344280324040, -17.24386586482343375, -219.6634241328915209 ) ) ;
#15522 = CARTESIAN_POINT ( 'NONE',  ( 9.333020543840051531, 16.91085096921651143, -217.7308990335875762 ) ) ;
#15523 = EDGE_CURVE ( 'NONE', #20366, #2937, #8566, .T. ) ;
#15524 = CARTESIAN_POINT ( 'NONE',  ( -10.84997096467605182, 25.01800101807719301, -232.4518260228253155 ) ) ;
#15525 = CIRCLE ( 'NONE', #20165, 3.000000000000002665 ) ;
#15526 = CARTESIAN_POINT ( 'NONE',  ( 22.66015888791822519, 10.43487984001084534, -234.3950629709119937 ) ) ;
#15527 = AXIS2_PLACEMENT_3D ( 'NONE', #4758, #9957, #1392 ) ;
#15528 = CARTESIAN_POINT ( 'NONE',  ( 1.217121169770782663, 15.31158828575123110, -230.6845728599757308 ) ) ;
#15529 = CARTESIAN_POINT ( 'NONE',  ( 0.09137847850201968880, 10.76827681573430517, 92.00000000000001421 ) ) ;
#15530 = CARTESIAN_POINT ( 'NONE',  ( -4.670971249126254499, -22.80666086768999890, -234.0323572959307512 ) ) ;
#15531 = CARTESIAN_POINT ( 'NONE',  ( 14.34945462593695531, -6.128426910066905542, -229.1128190117150041 ) ) ;
#15532 = CARTESIAN_POINT ( 'NONE',  ( 0.000000000000000000, 0.000000000000000000, -55.00000000000000711 ) ) ;
#15533 = DIRECTION ( 'NONE',  ( -1.000000000000000000, 0.000000000000000000, 0.000000000000000000 ) ) ;
#15534 = CARTESIAN_POINT ( 'NONE',  ( -15.39319649241581800, 0.3563955590804028795, -232.4397289486159082 ) ) ;
#15535 = CARTESIAN_POINT ( 'NONE',  ( -9.080867962954789263, -15.08739678120475780, -231.4478131780767001 ) ) ;
#15536 = CIRCLE ( 'NONE', #1148, 5.000000000000000888 ) ;
#15537 = CARTESIAN_POINT ( 'NONE',  ( 5.920190106170357680, -27.41802839654005197, -221.0732524667164114 ) ) ;
#15538 = CARTESIAN_POINT ( 'NONE',  ( -16.27882490622757672, 1.520697279646460398, -219.2607721384596289 ) ) ;
#15539 = CARTESIAN_POINT ( 'NONE',  ( 9.527502190795640757, 23.55559004943647139, -217.4101659741468211 ) ) ;
#15540 = CARTESIAN_POINT ( 'NONE',  ( 1.719513778997906694, 15.52930330544231730, -222.3959083836286368 ) ) ;
#15541 = VERTEX_POINT ( 'NONE', #5617 ) ;
#15542 = CARTESIAN_POINT ( 'NONE',  ( 27.25858960103340323, -9.764658377823966617, -217.2703135185301448 ) ) ;
#15543 = EDGE_LOOP ( 'NONE', ( #12115, #9289, #9326, #2079 ) ) ;
#15544 = CARTESIAN_POINT ( 'NONE',  ( 9.333020543840051531, 16.91085096921651143, -217.7308990335875762 ) ) ;
#15545 = EDGE_CURVE ( 'NONE', #12371, #15308, #4032, .T. ) ;
#15546 = TOROIDAL_SURFACE ( 'NONE', #9090, 16.23205080756887853, 2.000000000000000000 ) ;
#15547 = CARTESIAN_POINT ( 'NONE',  ( -24.30769394037691100, 17.48612956801762053, -223.4340414801748693 ) ) ;
#15548 = CARTESIAN_POINT ( 'NONE',  ( -15.72195651633673208, 2.938252489821347346, -222.2698596109374023 ) ) ;
#15549 = CARTESIAN_POINT ( 'NONE',  ( -15.43902962033193837, -12.71219713885795422, -232.7078469548986845 ) ) ;
#15550 = CARTESIAN_POINT ( 'NONE',  ( 14.99872922520050977, -2.000037915366065899, -222.7619559412280807 ) ) ;
#15551 = CARTESIAN_POINT ( 'NONE',  ( 26.59731715018858011, 13.56210517473685329, -229.5787264587298466 ) ) ;
#15552 = CARTESIAN_POINT ( 'NONE',  ( -15.77374768176864173, 20.07639682234129097, -218.6858893794192795 ) ) ;
#15553 = CARTESIAN_POINT ( 'NONE',  ( 14.96462366732929716, 7.179279272144128754, -233.2042342402542374 ) ) ;
#15554 = CARTESIAN_POINT ( 'NONE',  ( 15.88965480228581839, 12.37830464553330678, -233.8570207506254235 ) ) ;
#15555 = AXIS2_PLACEMENT_3D ( 'NONE', #16837, #4445, #18196 ) ;
#15556 = CARTESIAN_POINT ( 'NONE',  ( -15.42652243319914085, -1.944528292506083167, -233.0911082444762030 ) ) ;
#15557 = ORIENTED_EDGE ( 'NONE', *, *, #19718, .F. ) ;
#15558 = CARTESIAN_POINT ( 'NONE',  ( -4.902442737337177725, -13.94343087703807704, -224.3742458082145959 ) ) ;
#15559 = CARTESIAN_POINT ( 'NONE',  ( -20.38637754046084183, 19.95723714148678241, -217.5201383746364172 ) ) ;
#15560 = CARTESIAN_POINT ( 'NONE',  ( 9.358654279681809740, -11.94480763145079472, -229.8864256833185777 ) ) ;
#15561 = CARTESIAN_POINT ( 'NONE',  ( 2.837900457371055563, 25.11342719071438978, -232.9871906064174709 ) ) ;
#15562 = CARTESIAN_POINT ( 'NONE',  ( 15.97952439233267263, -1.339455371059026456, -231.0376074705642395 ) ) ;
#15563 = CARTESIAN_POINT ( 'NONE',  ( 25.50000000000000000, 0.000000000000000000, 0.000000000000000000 ) ) ;
#15564 = CARTESIAN_POINT ( 'NONE',  ( 16.48801037644500056, 3.165716804515234628, -216.8169430726136113 ) ) ;
#15565 = CYLINDRICAL_SURFACE ( 'NONE', #7034, 25.00000000000010303 ) ;
#15566 = CARTESIAN_POINT ( 'NONE',  ( -1.158668551263366986, 23.31492692626720853, -219.2372600964201865 ) ) ;
#15567 = CARTESIAN_POINT ( 'NONE',  ( -15.83178333309709629, 2.467763724635483324, -230.4064772870105458 ) ) ;
#15568 = CARTESIAN_POINT ( 'NONE',  ( 17.19674704922021391, 23.07334190050143974, -228.8256488842130238 ) ) ;
#15569 = CARTESIAN_POINT ( 'NONE',  ( 21.27683256847563698, 4.223177115764435108, -215.2584548172064842 ) ) ;
#15570 = CARTESIAN_POINT ( 'NONE',  ( 2.898952953659251985, -22.97888022809681274, -215.2852275949887826 ) ) ;
#15571 = CARTESIAN_POINT ( 'NONE',  ( 3.001892273201697048, 27.20292285420111966, -216.7800154582108689 ) ) ;
#15572 = AXIS2_PLACEMENT_3D ( 'NONE', #13192, #11280, #21394 ) ;
#15573 = AXIS2_PLACEMENT_3D ( 'NONE', #19560, #9340, #16526 ) ;
#15574 = CARTESIAN_POINT ( 'NONE',  ( 15.01439307471096463, 1.118969480519667048, -226.7488225241675366 ) ) ;
#15575 = CARTESIAN_POINT ( 'NONE',  ( -3.877698871368953082, -12.59008950621349676, -229.3284496285515388 ) ) ;
#15576 = CARTESIAN_POINT ( 'NONE',  ( -9.233762381136051189, 19.18161952504991419, -232.0796851897838451 ) ) ;
#15577 = CARTESIAN_POINT ( 'NONE',  ( 9.798337081649805214, 12.27506320122302697, -218.9346733583377613 ) ) ;
#15578 = EDGE_CURVE ( 'NONE', #8719, #20147, #18163, .T. ) ;
#15579 = CARTESIAN_POINT ( 'NONE',  ( -14.37894460687751597, -1.926260335694933268, -225.0161641904981593 ) ) ;
#15580 = CARTESIAN_POINT ( 'NONE',  ( -21.67128887413246119, 15.53484693247673043, -229.0088198863946900 ) ) ;
#15581 = CARTESIAN_POINT ( 'NONE',  ( -14.58670098223046629, 7.239570004716886942, -229.3284954533748135 ) ) ;
#15582 = CARTESIAN_POINT ( 'NONE',  ( 28.56567312134318826, 3.451746495494312672, -224.1550573921799412 ) ) ;
#15583 = ORIENTED_EDGE ( 'NONE', *, *, #7373, .T. ) ;
#15584 = CARTESIAN_POINT ( 'NONE',  ( 5.069241901512100412, 14.34986542013820632, -229.6420000777802954 ) ) ;
#15585 = CARTESIAN_POINT ( 'NONE',  ( 12.68099841568652764, -20.61692530233158394, -230.4218470428317573 ) ) ;
#15586 = ORIENTED_EDGE ( 'NONE', *, *, #16709, .T. ) ;
#15587 = CARTESIAN_POINT ( 'NONE',  ( 14.58943670538545412, -3.864781073802256550, -230.4050158740328129 ) ) ;
#15588 = CARTESIAN_POINT ( 'NONE',  ( -3.071946796551161984, 23.17078151772539485, -231.0066194318698933 ) ) ;
#15589 = CARTESIAN_POINT ( 'NONE',  ( 15.91295838535984331, 21.88410254487826379, -230.9583961155862823 ) ) ;
#15590 = CARTESIAN_POINT ( 'NONE',  ( -20.52308621596579030, -13.62600152083235905, -234.9101091540371442 ) ) ;
#15591 = CARTESIAN_POINT ( 'NONE',  ( 0.7326557587344989519, -29.96088689026728602, -229.4725774697800205 ) ) ;
#15592 = AXIS2_PLACEMENT_3D ( 'NONE', #880, #16195, #4351 ) ;
#15593 = CARTESIAN_POINT ( 'NONE',  ( 10.10435529162921853, -13.32996982371095918, -231.5224098423250894 ) ) ;
#15594 = AXIS2_PLACEMENT_3D ( 'NONE', #1873, #13825, #15733 ) ;
#15595 = CARTESIAN_POINT ( 'NONE',  ( -2.612157044224189484, 27.88031182936952135, -224.5292183073761692 ) ) ;
#15596 = DIRECTION ( 'NONE',  ( -0.000000000000000000, -1.000000000000000000, -0.000000000000000000 ) ) ;
#15597 = CARTESIAN_POINT ( 'NONE',  ( 15.33128967029630729, 6.504525012335983902, -229.0514072561169883 ) ) ;
#15598 = CARTESIAN_POINT ( 'NONE',  ( -11.46843428684449151, 6.508406145394057596, -225.7212143570321814 ) ) ;
#15599 = CARTESIAN_POINT ( 'NONE',  ( -14.98215928292561294, 22.79623052288931362, -230.3289734367122890 ) ) ;
#15600 = CARTESIAN_POINT ( 'NONE',  ( -24.76242154467160717, -4.839146110080178254, -231.6857664014047202 ) ) ;
#15601 = ORIENTED_EDGE ( 'NONE', *, *, #21369, .F. ) ;
#15602 = CARTESIAN_POINT ( 'NONE',  ( 2.951582164238582440, 19.39026647431845873, -217.4356918981242472 ) ) ;
#15603 = CARTESIAN_POINT ( 'NONE',  ( -24.82235633397527508, 10.76243500821901300, -227.9886044494091948 ) ) ;
#15604 = CARTESIAN_POINT ( 'NONE',  ( 15.51445714770079931, 9.275596138242290678, -215.8565574371285436 ) ) ;
#15605 = CARTESIAN_POINT ( 'NONE',  ( 4.999282783285113219, -13.99249059192112021, -223.3817383379047214 ) ) ;
#15606 = CARTESIAN_POINT ( 'NONE',  ( 1.387778780781445676E-13, -19.79999999999999716, 78.50000000000000000 ) ) ;
#15607 = ORIENTED_EDGE ( 'NONE', *, *, #5134, .F. ) ;
#15608 = CARTESIAN_POINT ( 'NONE',  ( -7.913358619554302642, 16.16796202616373890, -233.0981776325470491 ) ) ;
#15609 = CARTESIAN_POINT ( 'NONE',  ( 25.75976839005050323, -3.608312289253767347, -220.3697909415571417 ) ) ;
#15610 = CARTESIAN_POINT ( 'NONE',  ( 16.38151749656409351, 8.902090001712490874, -231.2955017965201989 ) ) ;
#15611 = CARTESIAN_POINT ( 'NONE',  ( -13.11494368899652052, 3.355507568391938200, -225.9121440085824304 ) ) ;
#15612 = CARTESIAN_POINT ( 'NONE',  ( 10.40291689048662782, -13.87512507945592333, -231.9656913702303029 ) ) ;
#15613 = CARTESIAN_POINT ( 'NONE',  ( -14.73016414256368911, 22.23431809695627237, -217.1425123644553707 ) ) ;
#15614 = CIRCLE ( 'NONE', #16735, 3.000000000000002665 ) ;
#15615 = CARTESIAN_POINT ( 'NONE',  ( 19.30248206944178335, -1.297331563427565726, -230.8957665284791290 ) ) ;
#15616 = CARTESIAN_POINT ( 'NONE',  ( -7.084830653876206696, -25.45310193036084456, -219.3007580301989492 ) ) ;
#15617 = DIRECTION ( 'NONE',  ( -1.000000000000000000, 0.000000000000000000, 0.000000000000000000 ) ) ;
#15618 = DIRECTION ( 'NONE',  ( -1.000000000000000000, 0.000000000000000000, 0.000000000000000000 ) ) ;
#15619 = CARTESIAN_POINT ( 'NONE',  ( -19.00318367631585659, 13.14621133775862916, -233.8403879275295765 ) ) ;
#15620 = CARTESIAN_POINT ( 'NONE',  ( 18.63320037895408277, -18.75851321891666146, -220.1409915463867151 ) ) ;
#15621 = CARTESIAN_POINT ( 'NONE',  ( 14.11699743667134399, -1.517512230688333963, -222.4120480544196994 ) ) ;
#15622 = CARTESIAN_POINT ( 'NONE',  ( -24.24718929195449135, 6.113767028403175985, 7.939869996053141143 ) ) ;
#15623 = CARTESIAN_POINT ( 'NONE',  ( 20.58393751692968721, 18.55948753678544705, -226.8933397075267635 ) ) ;
#15624 = ADVANCED_FACE ( 'NONE', ( #5721 ), #17782, .T. ) ;
#15625 = CARTESIAN_POINT ( 'NONE',  ( -5.298027976154672025, 13.43376398981453157, -220.6333279128949982 ) ) ;
#15626 = CARTESIAN_POINT ( 'NONE',  ( 20.90058474538433231, 18.60939544422136294, -225.8027644507526475 ) ) ;
#15627 = CARTESIAN_POINT ( 'NONE',  ( -3.190684129821126813, -24.11035010539542611, -218.3286195476113392 ) ) ;
#15628 = CARTESIAN_POINT ( 'NONE',  ( 24.71064586368820315, -12.65488197590634378, -232.9862317762581654 ) ) ;
#15629 = VERTEX_POINT ( 'NONE', #9233 ) ;
#15630 =( REPRESENTATION_RELATIONSHIP ('NONE','NONE', #5277, #21505 ) REPRESENTATION_RELATIONSHIP_WITH_TRANSFORMATION ( #12785 )SHAPE_REPRESENTATION_RELATIONSHIP( ) );
#15631 = CARTESIAN_POINT ( 'NONE',  ( 0.1556102272723409452, 19.71550568250159685, -232.1993058477363547 ) ) ;
#15632 = CARTESIAN_POINT ( 'NONE',  ( -21.10507617219916199, 14.90539259013048756, -229.7677326419877488 ) ) ;
#15633 = CARTESIAN_POINT ( 'NONE',  ( -19.59898341672158040, 3.279988180491820504, -234.9371679595475086 ) ) ;
#15634 = ORIENTED_EDGE ( 'NONE', *, *, #3156, .F. ) ;
#15635 = VECTOR ( 'NONE', #4609, 999.9999999999998863 ) ;
#15636 = CARTESIAN_POINT ( 'NONE',  ( -14.93084585968405875, -14.53813297593447373, -219.1962364975631772 ) ) ;
#15637 = LINE ( 'NONE', #17548, #8239 ) ;
#15638 = VERTEX_POINT ( 'NONE', #16093 ) ;
#15639 = CARTESIAN_POINT ( 'NONE',  ( 17.66865342763861690, 2.849170916951684784, -230.9175656266857004 ) ) ;
#15640 = CARTESIAN_POINT ( 'NONE',  ( 13.43702744235484303, -16.51261215982735209, -219.1853238157515875 ) ) ;
#15641 = CARTESIAN_POINT ( 'NONE',  ( 13.69275646168278371, 8.674223198772375909, -220.8699857572541987 ) ) ;
#15642 = CARTESIAN_POINT ( 'NONE',  ( -9.540790481621398200, 9.981116473660406996, -228.6478862620407995 ) ) ;
#15643 = CARTESIAN_POINT ( 'NONE',  ( 11.75404126451729070, 5.688294280104953415, -229.3533586468489602 ) ) ;
#15644 = CARTESIAN_POINT ( 'NONE',  ( 12.53674998645855787, 17.96979015029927851, -232.8843215672231679 ) ) ;
#15645 = DIRECTION ( 'NONE',  ( 0.000000000000000000, 0.000000000000000000, -1.000000000000000000 ) ) ;
#15646 = TOROIDAL_SURFACE ( 'NONE', #17446, 12.50000000000000355, 5.000000000000000000 ) ;
#15647 = CARTESIAN_POINT ( 'NONE',  ( 2.513843158659109456, -14.78137297724497401, -219.3443999184743518 ) ) ;
#15648 = AXIS2_PLACEMENT_3D ( 'NONE', #9079, #20767, #12231 ) ;
#15649 = CARTESIAN_POINT ( 'NONE',  ( 17.01060404384151781, -6.151862203644831162, -218.3248062500343849 ) ) ;
#15650 = DIRECTION ( 'NONE',  ( 0.000000000000000000, 0.000000000000000000, -1.000000000000000000 ) ) ;
#15651 = DIRECTION ( 'NONE',  ( 1.000000000000000000, 0.000000000000000000, 0.000000000000000000 ) ) ;
#15652 = CARTESIAN_POINT ( 'NONE',  ( -22.04004491965229207, 12.41871177236473578, -215.2165492276571115 ) ) ;
#15653 = CARTESIAN_POINT ( 'NONE',  ( -23.72332483825893235, -1.495203899552344007, -219.0564715008207770 ) ) ;
#15654 = CARTESIAN_POINT ( 'NONE',  ( 15.89621445970763070, 6.639162626453350313, -232.5295318698041456 ) ) ;
#15655 = CARTESIAN_POINT ( 'NONE',  ( 2.808299412262623473, 18.06245856371233316, -217.9832661743849656 ) ) ;
#15656 = CARTESIAN_POINT ( 'NONE',  ( -1.336753021691559962, 16.04398320409420720, -230.2310715620304507 ) ) ;
#15657 = EDGE_LOOP ( 'NONE', ( #4335, #7476 ) ) ;
#15658 = CARTESIAN_POINT ( 'NONE',  ( 15.13468687495441323, -1.603572186776826447, -217.3101985623318626 ) ) ;
#15659 = CARTESIAN_POINT ( 'NONE',  ( 27.40550551777678123, 5.967061366481472895, -228.7463788799179554 ) ) ;
#15660 = CARTESIAN_POINT ( 'NONE',  ( -11.01414002179357610, 8.614420160880040811, -226.3770540798392972 ) ) ;
#15661 = CARTESIAN_POINT ( 'NONE',  ( -13.48133478602219171, 10.24771958306113362, -218.3822527490931691 ) ) ;
#15662 = CARTESIAN_POINT ( 'NONE',  ( -6.776147227169700749, -16.68571135823561846, -231.0772860317820232 ) ) ;
#15663 = CARTESIAN_POINT ( 'NONE',  ( -18.08305592660031991, 4.022743421239192152, -217.2335041149100050 ) ) ;
#15664 = DIRECTION ( 'NONE',  ( 1.000000000000000000, 6.982962677686266711E-15, 0.000000000000000000 ) ) ;
#15665 = CIRCLE ( 'NONE', #3013, 19.80000000000007887 ) ;
#15666 = VECTOR ( 'NONE', #20154, 1000.000000000000000 ) ;
#15667 = CARTESIAN_POINT ( 'NONE',  ( 14.80781494020099132, -2.823191316056344657, -223.9669636951288965 ) ) ;
#15668 = CARTESIAN_POINT ( 'NONE',  ( 0.000000000000000000, 0.000000000000000000, 77.51594804401857175 ) ) ;
#15669 = CARTESIAN_POINT ( 'NONE',  ( -21.67128887413246119, 15.53484693247673043, -229.0088198863946900 ) ) ;
#15670 = CARTESIAN_POINT ( 'NONE',  ( 25.12984891811676036, 19.96069634721137476, -226.7154725927711070 ) ) ;
#15671 = CARTESIAN_POINT ( 'NONE',  ( -28.59157645096996347, 5.137867505054540374, -220.4667042235044505 ) ) ;
#15672 = CARTESIAN_POINT ( 'NONE',  ( -31.13345889576667247, -1.683779982087686422, -229.5421043233184264 ) ) ;
#15673 = ORIENTED_EDGE ( 'NONE', *, *, #5608, .F. ) ;
#15674 = CARTESIAN_POINT ( 'NONE',  ( -15.43902962033193837, -12.71219713885795422, -232.7078469548986845 ) ) ;
#15675 = CARTESIAN_POINT ( 'NONE',  ( -8.201407585998298444, 17.38801480109368924, -216.6295241303755006 ) ) ;
#15676 = CARTESIAN_POINT ( 'NONE',  ( -14.84823930505322132, -23.35465403802561823, -218.3226235040776260 ) ) ;
#15677 = CARTESIAN_POINT ( 'NONE',  ( 12.18657022793382794, 26.76558097653315471, -221.8882195427397335 ) ) ;
#15678 = CARTESIAN_POINT ( 'NONE',  ( 9.622280932921700725, -12.40415793303572300, -216.8820201732712860 ) ) ;
#15679 = CIRCLE ( 'NONE', #16050, 23.00000000000008882 ) ;
#15680 = PLANE ( 'NONE',  #3453 ) ;
#15681 =( GEOMETRIC_REPRESENTATION_CONTEXT ( 3 ) GLOBAL_UNCERTAINTY_ASSIGNED_CONTEXT ( ( #20200 ) ) GLOBAL_UNIT_ASSIGNED_CONTEXT ( ( #12296, #5750, #12630 ) ) REPRESENTATION_CONTEXT ( 'NONE', 'WORKASPACE' ) );
#15682 = CARTESIAN_POINT ( 'NONE',  ( -14.07336028695978314, 1.752429266630609828, -222.9750305084206161 ) ) ;
#15683 = CARTESIAN_POINT ( 'NONE',  ( -3.504118661534079582, 16.69899759879061918, -221.4378787282527128 ) ) ;
#15684 = CARTESIAN_POINT ( 'NONE',  ( -16.32047052250102581, 2.570795953410685009, -230.9329235942756213 ) ) ;
#15685 = CARTESIAN_POINT ( 'NONE',  ( -14.70339349403010942, -0.4153334646997780544, -217.8790668391084466 ) ) ;
#15686 = CARTESIAN_POINT ( 'NONE',  ( 15.14536540539411114, 2.907144070186200580, -217.8738854795238922 ) ) ;
#15687 = CARTESIAN_POINT ( 'NONE',  ( 2.374937041136545801, -21.24827930241302099, -215.2851479487023312 ) ) ;
#15688 = CARTESIAN_POINT ( 'NONE',  ( 6.523529190399725231, 13.69551997595937465, -217.3678933099786832 ) ) ;
#15689 = CARTESIAN_POINT ( 'NONE',  ( 14.98418162551161714, 4.450317369940187895, -227.9894155827521161 ) ) ;
#15690 = CARTESIAN_POINT ( 'NONE',  ( -3.265885032814331623, -11.59335615597398217, -224.1764024733101053 ) ) ;
#15691 = CARTESIAN_POINT ( 'NONE',  ( -5.365396334125453137, 16.47374957271378904, -219.4721119688156534 ) ) ;
#15692 = CIRCLE ( 'NONE', #6711, 19.00000000000000711 ) ;
#15693 = CARTESIAN_POINT ( 'NONE',  ( 14.69879291197755222, 10.86005690695417236, -216.7815908316746913 ) ) ;
#15694 = CARTESIAN_POINT ( 'NONE',  ( -15.46216926290318305, -2.495270579625169738, -221.2150947962298631 ) ) ;
#15695 = CARTESIAN_POINT ( 'NONE',  ( -22.36207348798144778, 17.12313795477538036, -223.8571857210765472 ) ) ;
#15696 = CARTESIAN_POINT ( 'NONE',  ( -10.01410430826631170, 16.10970239316000630, -233.6135099156378203 ) ) ;
#15697 = B_SPLINE_CURVE_WITH_KNOTS ( 'NONE', 3,
 ( #8631, #8963, #13924, #15491, #404, #7278, #14148, #20985, #14261, #19404 ),
 .UNSPECIFIED., .F., .F.,
 ( 4, 2, 2, 2, 4 ),
 ( 0.4921208414669437925, 0.4926212833915588618, 0.4960388740592901469, 0.4979917830122794764, 0.4999446919652688059 ),
 .UNSPECIFIED. ) ;
#15698 = CARTESIAN_POINT ( 'NONE',  ( 17.76485367938521875, 4.373152267827974171, -218.8623009891758215 ) ) ;
#15699 = ORIENTED_EDGE ( 'NONE', *, *, #10065, .F. ) ;
#15700 = CARTESIAN_POINT ( 'NONE',  ( 12.41447124200992391, -12.24348532208574269, -228.9129928441363973 ) ) ;
#15701 = ORIENTED_EDGE ( 'NONE', *, *, #9494, .T. ) ;
#15702 = CARTESIAN_POINT ( 'NONE',  ( 5.377793152941013233, -17.45375835550001753, -231.2474386379397231 ) ) ;
#15703 = CARTESIAN_POINT ( 'NONE',  ( -4.285397168228398890, 18.56782363833054106, -219.4990091916804715 ) ) ;
#15704 = VERTEX_POINT ( 'NONE', #5501 ) ;
#15705 =( NAMED_UNIT ( * ) PLANE_ANGLE_UNIT ( ) SI_UNIT ( $, .RADIAN. ) );
#15706 = CARTESIAN_POINT ( 'NONE',  ( 15.33737796850231305, 13.57479350230705428, -232.3313557812109025 ) ) ;
#15707 = CARTESIAN_POINT ( 'NONE',  ( 14.64930099072384095, -2.233284345536625803, -226.6630761355773984 ) ) ;
#15708 = CARTESIAN_POINT ( 'NONE',  ( -1.608171596096409806, -16.77465153034988887, -217.4618546331240054 ) ) ;
#15709 = CARTESIAN_POINT ( 'NONE',  ( 7.080148886126969465, -28.65852557119563926, -219.9679292432588227 ) ) ;
#15710 = CARTESIAN_POINT ( 'NONE',  ( -3.125843203957122896, 15.99774916147792680, -222.8808123721668721 ) ) ;
#15711 = CARTESIAN_POINT ( 'NONE',  ( 0.000000000000000000, 23.00000000000006040, -24.99999999999999289 ) ) ;
#15712 = CARTESIAN_POINT ( 'NONE',  ( 25.18311526135610734, 13.65721788432563955, -224.7326014392022273 ) ) ;
#15713 = CARTESIAN_POINT ( 'NONE',  ( -10.30050448363967419, 10.07750059423401190, -220.1837019037183723 ) ) ;
#15714 = CARTESIAN_POINT ( 'NONE',  ( -3.504118661534079582, 16.69899759879061918, -221.4378787282527128 ) ) ;
#15715 = EDGE_CURVE ( 'NONE', #15877, #137, #9192, .T. ) ;
#15716 = CARTESIAN_POINT ( 'NONE',  ( 1.656472371294090085, 27.29382523973669095, -230.4991099578876117 ) ) ;
#15717 = CARTESIAN_POINT ( 'NONE',  ( -17.72669652144150376, 1.460525322529694581, -220.6883622781615202 ) ) ;
#15718 = CARTESIAN_POINT ( 'NONE',  ( 9.169328349715531346, 20.85917603618721472, -214.7000934853629133 ) ) ;
#15719 = CARTESIAN_POINT ( 'NONE',  ( 6.025688374458400887, -15.61258154445926749, -220.0079782759978002 ) ) ;
#15720 = DIRECTION ( 'NONE',  ( -0.000000000000000000, -1.000000000000000000, -0.000000000000000000 ) ) ;
#15721 = VERTEX_POINT ( 'NONE', #342 ) ;
#15722 = CARTESIAN_POINT ( 'NONE',  ( -3.673551555920188783, 29.81207051619892923, -228.8770490300152005 ) ) ;
#15723 = CARTESIAN_POINT ( 'NONE',  ( -27.90711606799872513, 0.4679914357742857023, -216.8754026763949128 ) ) ;
#15724 = CARTESIAN_POINT ( 'NONE',  ( 28.33476664927451338, -0.7768526459456059907, -228.3750448408243869 ) ) ;
#15725 = CARTESIAN_POINT ( 'NONE',  ( 18.60971343765040942, 2.368090295052050820, -218.6871071987073094 ) ) ;
#15726 = CARTESIAN_POINT ( 'NONE',  ( -21.93900267957129557, 7.862893636934532360, -233.4951761057262161 ) ) ;
#15727 = CARTESIAN_POINT ( 'NONE',  ( 2.378655016347637652, -14.31292064579845302, -219.9942319014987220 ) ) ;
#15728 = CARTESIAN_POINT ( 'NONE',  ( -8.172572110426221670, 16.86653848210977813, -233.4220330256369493 ) ) ;
#15729 = CARTESIAN_POINT ( 'NONE',  ( -11.59479561055411345, 9.544396733298208702, -229.1494558965577255 ) ) ;
#15730 = EDGE_LOOP ( 'NONE', ( #5585, #14240, #7392, #7220 ) ) ;
#15731 = CARTESIAN_POINT ( 'NONE',  ( -29.88125065636863198, 4.504452993877526623, -226.2048141718237275 ) ) ;
#15732 = CARTESIAN_POINT ( 'NONE',  ( -8.983992482398329926, -13.08794618741998761, -229.3325301586503713 ) ) ;
#15733 = DIRECTION ( 'NONE',  ( 0.000000000000000000, 0.000000000000000000, 1.000000000000000000 ) ) ;
#15734 = CARTESIAN_POINT ( 'NONE',  ( -25.00000000000000000, 3.061616997868383043E-15, 75.00000000000000000 ) ) ;
#15735 = CARTESIAN_POINT ( 'NONE',  ( -17.79285498209129202, 9.187865686019035749, -216.3798185811636756 ) ) ;
#15736 = CARTESIAN_POINT ( 'NONE',  ( 1.345830553852720657, -29.56269728401072783, -219.9360760428637604 ) ) ;
#15737 = SURFACE_STYLE_FILL_AREA ( #4118 ) ;
#15738 = CARTESIAN_POINT ( 'NONE',  ( -23.84163028481813029, 7.537079486365330538, 6.604381661968267814 ) ) ;
#15739 = CARTESIAN_POINT ( 'NONE',  ( 17.51175949430614409, 14.31829016556564937, -218.8195841045835550 ) ) ;
#15740 = CARTESIAN_POINT ( 'NONE',  ( -4.450022810944913587, 12.45400981846350597, -225.2098051417536340 ) ) ;
#15741 = DIRECTION ( 'NONE',  ( 0.000000000000000000, 0.000000000000000000, -1.000000000000000000 ) ) ;
#15742 = CARTESIAN_POINT ( 'NONE',  ( 15.88536911906737181, 12.85343532334862893, -218.9532478288372204 ) ) ;
#15743 = CARTESIAN_POINT ( 'NONE',  ( 4.746237488610151267, -29.30821474977460639, -222.1257927337785247 ) ) ;
#15745 = ADVANCED_FACE ( 'NONE', ( #7210 ), #21134, .F. ) ;
#15744 = CARTESIAN_POINT ( 'NONE',  ( 23.77009720158773831, -0.5966687509537305090, -216.6384684467892043 ) ) ;
#15746 = VERTEX_POINT ( 'NONE', #13856 ) ;
#15747 = CARTESIAN_POINT ( 'NONE',  ( -4.224287562409271501, 29.03635716824519264, -224.1823526280761882 ) ) ;
#15748 = CARTESIAN_POINT ( 'NONE',  ( -24.48812334466693486, 4.469247780253509106, -230.3044243311433945 ) ) ;
#15749 = CARTESIAN_POINT ( 'NONE',  ( -11.84805200323110164, 5.835720598137266180, -228.2740675967047537 ) ) ;
#15750 = CARTESIAN_POINT ( 'NONE',  ( -22.39763175122653038, -14.70415172796113623, -221.0757120432126612 ) ) ;
#15751 = CARTESIAN_POINT ( 'NONE',  ( 0.000000000000000000, 0.000000000000000000, 75.00000000000000000 ) ) ;
#15752 = VERTEX_POINT ( 'NONE', #20696 ) ;
#15753 = CARTESIAN_POINT ( 'NONE',  ( 17.81160404892403193, 9.939217752910943560, -216.9646549374535311 ) ) ;
#15754 = CARTESIAN_POINT ( 'NONE',  ( 0.005738405568439595983, -15.19016956849912070, -227.2100150994057230 ) ) ;
#15755 = CARTESIAN_POINT ( 'NONE',  ( 10.55627441269396094, 10.31758739525044888, -223.1990319438957613 ) ) ;
#15756 = CARTESIAN_POINT ( 'NONE',  ( -17.65835845419170624, 22.55329142274348442, -231.2673511165784532 ) ) ;
#15757 = ADVANCED_FACE ( 'NONE', ( #12601, #5273 ), #12154, .T. ) ;
#15758 = CARTESIAN_POINT ( 'NONE',  ( 14.81258087342262364, 2.398747990731791013, -230.9000679928271040 ) ) ;
#15759 = CARTESIAN_POINT ( 'NONE',  ( 2.837900457371055563, 25.11342719071438978, -232.9871906064174709 ) ) ;
#15760 = CARTESIAN_POINT ( 'NONE',  ( 15.26418234037447164, 1.657826554291933485, -222.4969140426460683 ) ) ;
#15761 = EDGE_CURVE ( 'NONE', #10560, #7254, #901, .T. ) ;
#15762 = CARTESIAN_POINT ( 'NONE',  ( -1.633632075387274840, -15.48245080501611071, -218.5193615163172751 ) ) ;
#15763 = CARTESIAN_POINT ( 'NONE',  ( 22.14671607713456325, -14.13547298543019437, -218.1897693226341914 ) ) ;
#15764 = DIRECTION ( 'NONE',  ( 1.000000000000000000, -0.000000000000000000, -0.000000000000000000 ) ) ;
#15765 = DIRECTION ( 'NONE',  ( 1.000000000000000000, 0.000000000000000000, 0.000000000000000000 ) ) ;
#15766 = CARTESIAN_POINT ( 'NONE',  ( -9.491065840222427497, 13.31995980477872266, -232.8537120564120073 ) ) ;
#15767 = CARTESIAN_POINT ( 'NONE',  ( -27.87965705189043675, -2.801641921304233840, -225.5825458398584260 ) ) ;
#15768 = CARTESIAN_POINT ( 'NONE',  ( 17.34461553379066601, 6.893916422670210764, -233.3442385185644525 ) ) ;
#15769 = CARTESIAN_POINT ( 'NONE',  ( 5.803912621764987456, 13.01725692290267844, -221.8367675400179166 ) ) ;
#15770 = CARTESIAN_POINT ( 'NONE',  ( -2.043230952238195286, 23.63069326910348877, -232.6835180461029040 ) ) ;
#15771 = ORIENTED_EDGE ( 'NONE', *, *, #10238, .T. ) ;
#15772 = CARTESIAN_POINT ( 'NONE',  ( 13.13237050162318553, -11.26662123460813092, -216.1773046078333209 ) ) ;
#15773 = EDGE_LOOP ( 'NONE', ( #12033, #17829 ) ) ;
#15774 = CARTESIAN_POINT ( 'NONE',  ( 27.75679124201660741, 4.911524026080384075, -221.4430403652340829 ) ) ;
#15775 = CARTESIAN_POINT ( 'NONE',  ( -13.63002737749749826, 6.315035547785179837, -227.0490028799284516 ) ) ;
#15776 = CARTESIAN_POINT ( 'NONE',  ( -11.94727018630768178, 9.025563988971828877, -220.6148682757971358 ) ) ;
#15777 = CARTESIAN_POINT ( 'NONE',  ( -28.43596199216294806, -10.51226423640377838, -227.0041752157952430 ) ) ;
#15778 = CARTESIAN_POINT ( 'NONE',  ( -13.55591840520136770, 8.363404288414606924, -231.2690188357804857 ) ) ;
#15779 = CIRCLE ( 'NONE', #3523, 23.00000000000000000 ) ;
#15780 = DIRECTION ( 'NONE',  ( -2.891205793294678696E-17, 0.000000000000000000, -1.000000000000000000 ) ) ;
#15781 = CARTESIAN_POINT ( 'NONE',  ( -25.52219491023488018, 3.125567430403401865E-15, 89.47905546699919910 ) ) ;
#15782 = CARTESIAN_POINT ( 'NONE',  ( 14.50618777373884960, 4.375057440872940795, -230.8807389798650433 ) ) ;
#15783 = CARTESIAN_POINT ( 'NONE',  ( -18.59263364681495290, 22.28600439725833482, -224.9897462721271779 ) ) ;
#15784 = CARTESIAN_POINT ( 'NONE',  ( 5.784594921161807513, 11.98867617302893329, -219.3746160931291058 ) ) ;
#15785 = CARTESIAN_POINT ( 'NONE',  ( 20.54442553493903389, -1.409480604460696007, -231.2888200459364327 ) ) ;
#15786 = CARTESIAN_POINT ( 'NONE',  ( -17.45568254742804370, -7.678338623619185732, -234.9220303918225738 ) ) ;
#15787 = CARTESIAN_POINT ( 'NONE',  ( -29.05925532287432489, -3.238226816112620199, -230.1495230746535867 ) ) ;
#15788 = CARTESIAN_POINT ( 'NONE',  ( -21.64120863631820413, 17.87363223393748868, -233.1390268986752119 ) ) ;
#15789 = CARTESIAN_POINT ( 'NONE',  ( -15.46269062504165781, -26.67469327287815517, -225.2085449711190677 ) ) ;
#15790 = CARTESIAN_POINT ( 'NONE',  ( 7.769483725421269860, 20.68783433326350263, -233.2348178266662728 ) ) ;
#15791 = CARTESIAN_POINT ( 'NONE',  ( 7.023652882903417272, -9.473209335044964874, -223.0206350579724983 ) ) ;
#15792 = DIRECTION ( 'NONE',  ( 1.000000000000000000, 0.000000000000000000, 0.000000000000000000 ) ) ;
#15793 = CARTESIAN_POINT ( 'NONE',  ( -22.13857085231108712, 6.545953331035805789, -217.2801712530867633 ) ) ;
#15794 = CARTESIAN_POINT ( 'NONE',  ( 0.000000000000000000, 0.000000000000000000, -75.05807060175870049 ) ) ;
#15795 = CARTESIAN_POINT ( 'NONE',  ( 1.030230143518703345, 18.27887886751213387, -229.5791973322770616 ) ) ;
#15796 = CARTESIAN_POINT ( 'NONE',  ( 12.47670316482120967, 2.249148913447538423, -227.4574095259895898 ) ) ;
#15797 = CARTESIAN_POINT ( 'NONE',  ( 20.34032485158648029, 2.741617426884598530, -217.9827731991294968 ) ) ;
#15798 = CARTESIAN_POINT ( 'NONE',  ( 26.75666476377482539, 8.100664119735744961, -232.1611550320539834 ) ) ;
#15799 = CARTESIAN_POINT ( 'NONE',  ( -9.080867962954789263, -15.08739678120475780, -231.4478131780767001 ) ) ;
#15800 = CARTESIAN_POINT ( 'NONE',  ( 2.068961274655788607, 15.13167107497539376, -217.8084559455312501 ) ) ;
#15801 = CYLINDRICAL_SURFACE ( 'NONE', #18432, 17.50000000000000355 ) ;
#15802 = CARTESIAN_POINT ( 'NONE',  ( 0.3659801352207852077, -13.50984377477715093, -221.1746532791751463 ) ) ;
#15803 = CARTESIAN_POINT ( 'NONE',  ( -4.742143146070755932, 15.01230778631049567, -221.4832709320255049 ) ) ;
#15804 = CARTESIAN_POINT ( 'NONE',  ( 9.211411085256067111, 16.86455563410128633, -232.8411836211112700 ) ) ;
#15805 = CARTESIAN_POINT ( 'NONE',  ( -26.22594988380878789, -0.1068133454905619700, -219.1167922977186322 ) ) ;
#15806 = CARTESIAN_POINT ( 'NONE',  ( -15.07599795178976443, 12.40109266655585429, -218.9921934537110815 ) ) ;
#15807 = CARTESIAN_POINT ( 'NONE',  ( -6.111257124579617894, 15.89946952501658295, -216.3497764690875727 ) ) ;
#15808 = CARTESIAN_POINT ( 'NONE',  ( 27.58248235015124550, 10.80791576765187934, -226.6933256641281389 ) ) ;
#15809 = VERTEX_POINT ( 'NONE', #19011 ) ;
#15810 = CARTESIAN_POINT ( 'NONE',  ( 6.772180301198498675, -16.47206380092378097, -229.1778777248402719 ) ) ;
#15811 = ORIENTED_EDGE ( 'NONE', *, *, #11620, .T. ) ;
#15812 = CARTESIAN_POINT ( 'NONE',  ( 13.60960062514055657, -26.18013421850907108, -225.9721930653775246 ) ) ;
#15813 = CARTESIAN_POINT ( 'NONE',  ( -2.426309470044460959, 27.69042070294474556, -223.4541227565655674 ) ) ;
#15814 = CARTESIAN_POINT ( 'NONE',  ( 11.67669251569587985, 24.04736029062789981, -218.5856804285192254 ) ) ;
#15815 = CARTESIAN_POINT ( 'NONE',  ( 16.50235023187294203, -3.000022380394500310, -230.0447763498268614 ) ) ;
#15816 = CARTESIAN_POINT ( 'NONE',  ( -24.15031621174628285, -13.05338392360020627, -219.0842748323915714 ) ) ;
#15817 = CARTESIAN_POINT ( 'NONE',  ( -4.670971249126254499, -22.80666086768999890, -234.0323572959307512 ) ) ;
#15818 = CARTESIAN_POINT ( 'NONE',  ( -2.426309470044460959, 27.69042070294474556, -223.4541227565655674 ) ) ;
#15819 = DIRECTION ( 'NONE',  ( -1.000000000000000000, 0.000000000000000000, 0.000000000000000000 ) ) ;
#15820 = CARTESIAN_POINT ( 'NONE',  ( 20.58393751692968721, 18.55948753678544705, -226.8933397075267635 ) ) ;
#15821 = CARTESIAN_POINT ( 'NONE',  ( -18.39892766464214446, 25.11039525536027739, -225.3444503920457294 ) ) ;
#15822 = CARTESIAN_POINT ( 'NONE',  ( -12.33997807949817904, 15.01940705987184188, -217.6798968600957380 ) ) ;
#15823 = CARTESIAN_POINT ( 'NONE',  ( 3.312424284731937618, 15.29837714273186045, -229.5209971419123747 ) ) ;
#15824 = CARTESIAN_POINT ( 'NONE',  ( -16.54465188417290022, 6.134005835925411709, -228.8256222654843270 ) ) ;
#15825 = CARTESIAN_POINT ( 'NONE',  ( 28.77543668145700195, 2.466904630248945907, -219.6646827587300947 ) ) ;
#15826 = CARTESIAN_POINT ( 'NONE',  ( 18.70674991763376482, -20.04093309878971496, -230.8534322170362714 ) ) ;
#15827 = DIRECTION ( 'NONE',  ( 0.000000000000000000, -1.000000000000000000, 0.000000000000000000 ) ) ;
#15828 = ORIENTED_EDGE ( 'NONE', *, *, #17961, .F. ) ;
#15829 = EDGE_CURVE ( 'NONE', #15223, #6741, #1982, .T. ) ;
#15830 = CARTESIAN_POINT ( 'NONE',  ( 4.730976410881341465, 17.65764351829336931, -217.6025626048331674 ) ) ;
#15831 = CARTESIAN_POINT ( 'NONE',  ( 15.95205345792057550, -4.116367354408478896, -227.2937718740910498 ) ) ;
#15832 = CARTESIAN_POINT ( 'NONE',  ( 16.06750045776299629, -1.909440863493336860, -220.4398626676318713 ) ) ;
#15833 = CARTESIAN_POINT ( 'NONE',  ( 14.32085100525799248, 9.220655089380342062, -219.9006227404039464 ) ) ;
#15834 = CARTESIAN_POINT ( 'NONE',  ( 6.166782020495575445, -26.61202787628535660, -217.6604608484729795 ) ) ;
#15835 = CARTESIAN_POINT ( 'NONE',  ( 0.000000000000000000, 0.000000000000000000, 0.000000000000000000 ) ) ;
#15836 = CARTESIAN_POINT ( 'NONE',  ( -11.69688825528096388, 18.63404371591177622, -215.8612738028812714 ) ) ;
#15837 = CARTESIAN_POINT ( 'NONE',  ( -12.30606003331388543, 10.59782772616791036, -231.0021630509705801 ) ) ;
#15838 = ORIENTED_EDGE ( 'NONE', *, *, #17864, .F. ) ;
#15839 = CARTESIAN_POINT ( 'NONE',  ( -19.25929423112888017, 9.818144317380269825, -216.1837936240308409 ) ) ;
#15840 = CARTESIAN_POINT ( 'NONE',  ( -24.09642229725868745, -17.04339013636034750, -228.1169379854252384 ) ) ;
#15841 = CARTESIAN_POINT ( 'NONE',  ( -24.97326975762673840, -1.324061100770212773, -9.933696595364846615 ) ) ;
#15842 = CARTESIAN_POINT ( 'NONE',  ( -22.77738497769248127, 3.250935496930576818, 9.479599941460891799 ) ) ;
#15843 = CARTESIAN_POINT ( 'NONE',  ( -21.02719846458807851, 18.12262440796364871, -218.0220709499931502 ) ) ;
#15844 = CARTESIAN_POINT ( 'NONE',  ( 7.434033643350927534, -13.76500825175950027, -228.7793665183827159 ) ) ;
#15845 =( LENGTH_UNIT ( ) NAMED_UNIT ( * ) SI_UNIT ( .MILLI., .METRE. ) );
#15846 = CARTESIAN_POINT ( 'NONE',  ( -24.11365241543554916, 6.615335895425515034, 7.527466726025860311 ) ) ;
#15847 = CARTESIAN_POINT ( 'NONE',  ( 15.04029996350473830, 7.457450192165341107, -220.5007084872782173 ) ) ;
#15848 = CARTESIAN_POINT ( 'NONE',  ( -6.079211283031130897, 16.94466709905296753, -232.9163774423793711 ) ) ;
#15849 = FACE_OUTER_BOUND ( 'NONE', #20703, .T. ) ;
#15850 = CARTESIAN_POINT ( 'NONE',  ( 11.87550186346493497, 14.27797038184677270, -220.2068243228838185 ) ) ;
#15851 = CARTESIAN_POINT ( 'NONE',  ( 3.303203443418958773, -15.45560242990989686, -230.9065799468681917 ) ) ;
#15852 = ORIENTED_EDGE ( 'NONE', *, *, #989, .T. ) ;
#15853 = CARTESIAN_POINT ( 'NONE',  ( -1.433739110790628102, 17.19322394474796667, -219.1420620387681879 ) ) ;
#15854 = CARTESIAN_POINT ( 'NONE',  ( -18.64931821476190876, 22.04453097546810270, -226.2485927806324923 ) ) ;
#15855 = CARTESIAN_POINT ( 'NONE',  ( -13.84508897751235246, 5.904954704487344941, -218.7722818424232401 ) ) ;
#15856 = CARTESIAN_POINT ( 'NONE',  ( -15.48718561803335625, -8.207282836869444154, -229.3046138068065147 ) ) ;
#15857 = CARTESIAN_POINT ( 'NONE',  ( 24.63401512838748530, 0.000000000000000000, -77.51594804401857175 ) ) ;
#15858 = ORIENTED_EDGE ( 'NONE', *, *, #19516, .T. ) ;
#15859 = CARTESIAN_POINT ( 'NONE',  ( 13.15438416660314225, 5.520603777723624539, -227.0878346348094681 ) ) ;
#15860 = CARTESIAN_POINT ( 'NONE',  ( 1.312189596842585404, -27.84482500255423432, -221.0181370286903473 ) ) ;
#15861 = CARTESIAN_POINT ( 'NONE',  ( 18.50911814746675788, 15.92944434255054453, -232.0449215596906072 ) ) ;
#15862 = CARTESIAN_POINT ( 'NONE',  ( -23.98802705797876200, 19.46654170242919690, -223.5293093576406989 ) ) ;
#15863 = CARTESIAN_POINT ( 'NONE',  ( 15.06072304412464291, 3.291435955319735651, -218.8606307204261725 ) ) ;
#15864 = ADVANCED_FACE ( 'NONE', ( #17665 ), #17328, .F. ) ;
#15865 = CARTESIAN_POINT ( 'NONE',  ( 1.382955251742491898, 16.46353944795171032, -231.7743150979565030 ) ) ;
#15866 = CARTESIAN_POINT ( 'NONE',  ( 2.000000000000000000, 0.000000000000000000, -105.0000000000000142 ) ) ;
#15867 = CARTESIAN_POINT ( 'NONE',  ( -14.24095617957673632, -25.86326826095433162, -229.7068514753157160 ) ) ;
#15868 = CARTESIAN_POINT ( 'NONE',  ( 11.31395536621571019, -8.070181239749643964, -225.0898076798974614 ) ) ;
#15869 = DIRECTION ( 'NONE',  ( -1.000000000000000000, 0.000000000000000000, 0.000000000000000000 ) ) ;
#15870 = DIRECTION ( 'NONE',  ( -1.000000000000000000, 0.000000000000000000, 0.000000000000000000 ) ) ;
#15871 = CARTESIAN_POINT ( 'NONE',  ( -19.40752943788874774, 15.61499612050012864, -234.7624367253776541 ) ) ;
#15872 = CARTESIAN_POINT ( 'NONE',  ( -19.42704602366333688, -5.151203963165301936, -219.4215732619585708 ) ) ;
#15873 = EDGE_CURVE ( 'NONE', #22262, #13805, #10265, .T. ) ;
#15874 = CARTESIAN_POINT ( 'NONE',  ( -23.20103936322198024, 10.64725167743880085, -231.7714206262400864 ) ) ;
#15875 = CARTESIAN_POINT ( 'NONE',  ( 1.104227501629593045, 25.05528885094460989, -231.9808705443460326 ) ) ;
#15876 = CARTESIAN_POINT ( 'NONE',  ( -1.707778556226592581, 19.51307486516442680, -232.5708079709245055 ) ) ;
#15877 = VERTEX_POINT ( 'NONE', #12381 ) ;
#15878 = CARTESIAN_POINT ( 'NONE',  ( 13.14132348467506439, -13.49276336982165780, -234.5843434792288633 ) ) ;
#15879 = ORIENTED_EDGE ( 'NONE', *, *, #7546, .F. ) ;
#15880 = CARTESIAN_POINT ( 'NONE',  ( 13.49011766416699842, 7.659170998773840111, -228.1905628957712793 ) ) ;
#15881 = CARTESIAN_POINT ( 'NONE',  ( -18.70090456008720992, 23.36146401084868884, -220.3989740370807056 ) ) ;
#15882 = CARTESIAN_POINT ( 'NONE',  ( -23.30382222616342247, 9.914163031146200566, -218.5285240371296425 ) ) ;
#15883 = CARTESIAN_POINT ( 'NONE',  ( -14.28784611495131784, -7.281039336628973402, -230.6208668958216208 ) ) ;
#15884 = CARTESIAN_POINT ( 'NONE',  ( -27.29953305526601426, 11.21644211419729054, -229.3676346105362995 ) ) ;
#15885 = CARTESIAN_POINT ( 'NONE',  ( -24.63401512838747820, 0.000000000000000000, 77.51594804401857175 ) ) ;
#15886 = CARTESIAN_POINT ( 'NONE',  ( 22.42925200799500729, 5.652256920629083581, -234.0734181799116698 ) ) ;
#15887 = AXIS2_PLACEMENT_3D ( 'NONE', #12883, #4424, #21638 ) ;
#15888 = CARTESIAN_POINT ( 'NONE',  ( -8.892156391762910062, 11.89593067802204551, -225.4519868197583889 ) ) ;
#15889 = CARTESIAN_POINT ( 'NONE',  ( 25.17176037151762813, 18.95054595444721102, -221.3490360113488862 ) ) ;
#15890 = CARTESIAN_POINT ( 'NONE',  ( -28.17543631911187063, 3.557555778861649642, -230.1980773687482156 ) ) ;
#15891 = CARTESIAN_POINT ( 'NONE',  ( -14.65326448616001898, -2.737518208283025167, -217.6605647598149744 ) ) ;
#15892 = CIRCLE ( 'NONE', #14815, 21.80000000000000071 ) ;
#15893 = CARTESIAN_POINT ( 'NONE',  ( -18.41550138691291139, -5.273244084890690075, -216.7348800533310964 ) ) ;
#15894 = CARTESIAN_POINT ( 'NONE',  ( -1.238249567024760189, 29.30580384236933966, -223.2399636023643836 ) ) ;
#15895 = CARTESIAN_POINT ( 'NONE',  ( -13.60146639818222702, -25.11808310587244009, -230.9974232610874196 ) ) ;
#15896 = CARTESIAN_POINT ( 'NONE',  ( 12.10245006109274080, 26.02147364279441888, -220.6079829738538649 ) ) ;
#15897 = CARTESIAN_POINT ( 'NONE',  ( 14.71544223636061410, -24.97731814513734605, -232.6985170686097320 ) ) ;
#15898 = CARTESIAN_POINT ( 'NONE',  ( 0.000000000000000000, -17.50000000000001066, -30.00000000000000000 ) ) ;
#15899 = CARTESIAN_POINT ( 'NONE',  ( 25.30228294196351868, 7.987863777258004561, -233.0744943826964573 ) ) ;
#15900 = DIRECTION ( 'NONE',  ( -0.000000000000000000, -0.000000000000000000, -1.000000000000000000 ) ) ;
#15901 = EDGE_CURVE ( 'NONE', #2965, #3572, #19117, .T. ) ;
#15902 = CARTESIAN_POINT ( 'NONE',  ( -8.316066124693966444, 26.67103469786491843, -222.2304303634109885 ) ) ;
#15903 = CARTESIAN_POINT ( 'NONE',  ( 29.01678366425524658, 8.126504218505314014, -229.6975090854573125 ) ) ;
#15904 = AXIS2_PLACEMENT_3D ( 'NONE', #21584, #2899, #6065 ) ;
#15905 = CARTESIAN_POINT ( 'NONE',  ( 28.02123297569005089, 5.903198806000402143, -227.5759114383273811 ) ) ;
#15906 = CARTESIAN_POINT ( 'NONE',  ( -24.15814485343234352, 4.373587128574028426, -232.6698675874553430 ) ) ;
#15907 = CARTESIAN_POINT ( 'NONE',  ( -12.55242351043508542, -12.71283815946331686, -230.7436264644880737 ) ) ;
#15908 = CARTESIAN_POINT ( 'NONE',  ( 11.20713200305815427, 28.28922876448651635, -219.1239564724620834 ) ) ;
#15909 = CARTESIAN_POINT ( 'NONE',  ( 2.465190328815681510E-29, 21.63401512838760610, 77.51594804401857175 ) ) ;
#15910 = CARTESIAN_POINT ( 'NONE',  ( -8.649444225544010934, -13.15555178350489918, -216.8547715670961509 ) ) ;
#15911 = CARTESIAN_POINT ( 'NONE',  ( -4.784012432433236484, 23.31984772163034947, -232.0554186943449508 ) ) ;
#15912 = AXIS2_PLACEMENT_3D ( 'NONE', #19859, #18084, #9534 ) ;
#15913 = CARTESIAN_POINT ( 'NONE',  ( 6.771176146757415637, 15.60014285904435027, -218.3493856697694753 ) ) ;
#15914 = AXIS2_PLACEMENT_3D ( 'NONE', #1692, #18580, #6758 ) ;
#15915 = CARTESIAN_POINT ( 'NONE',  ( -12.04619960554013502, 10.22290173510000777, -223.1766370265664534 ) ) ;
#15916 = CARTESIAN_POINT ( 'NONE',  ( -4.424820997438546399, 11.84746159238278373, -221.7815792475208525 ) ) ;
#15917 = CARTESIAN_POINT ( 'NONE',  ( 15.07212457412616224, 2.472408313530222390, -227.3472192494155024 ) ) ;
#15918 = CARTESIAN_POINT ( 'NONE',  ( 13.51502823286059929, -13.46037062290453790, -230.3041566501836144 ) ) ;
#15919 = ORIENTED_EDGE ( 'NONE', *, *, #22048, .F. ) ;
#15920 = CARTESIAN_POINT ( 'NONE',  ( 11.64632602964496044, -20.35392056169815689, -232.5450580586399383 ) ) ;
#15921 = CARTESIAN_POINT ( 'NONE',  ( -3.139695637132168038, 25.12735071829084177, -230.1469660918596389 ) ) ;
#15922 = DIRECTION ( 'NONE',  ( 0.000000000000000000, 0.000000000000000000, -1.000000000000000000 ) ) ;
#15923 = CARTESIAN_POINT ( 'NONE',  ( 18.29617186523616468, 23.20920553663278341, -223.4372550713720216 ) ) ;
#15924 = CARTESIAN_POINT ( 'NONE',  ( 15.05575868828727515, -2.428864548505686560, -227.9368649688638584 ) ) ;
#15925 = CARTESIAN_POINT ( 'NONE',  ( -13.33530847390368024, -5.065163879519744228, -226.5386329521395226 ) ) ;
#15926 = CARTESIAN_POINT ( 'NONE',  ( -1.890995374385051608, -13.09686096954197509, -227.5694739903412085 ) ) ;
#15927 = CARTESIAN_POINT ( 'NONE',  ( 1.296323513242173542, 20.09034598902932345, -230.5712631353794961 ) ) ;
#15928 = LINE ( 'NONE', #14460, #2609 ) ;
#15929 = CARTESIAN_POINT ( 'NONE',  ( 14.37653162493774239, 9.985418694807894013, -229.1686718965858063 ) ) ;
#15930 = EDGE_CURVE ( 'NONE', #9167, #7333, #8474, .T. ) ;
#15931 = CARTESIAN_POINT ( 'NONE',  ( -10.51143808951550085, 11.41308718311005066, -231.3573069600382439 ) ) ;
#15932 = CARTESIAN_POINT ( 'NONE',  ( -15.33438615632468149, 23.56248205204123991, -229.2747191038674544 ) ) ;
#15933 = VERTEX_POINT ( 'NONE', #12264 ) ;
#15934 = VECTOR ( 'NONE', #21005, 1000.000000000000000 ) ;
#15935 = VECTOR ( 'NONE', #18557, 1000.000000000000000 ) ;
#15936 = CARTESIAN_POINT ( 'NONE',  ( 6.566035546683759883, 15.06745272174450712, -218.8330720708048034 ) ) ;
#15937 = CARTESIAN_POINT ( 'NONE',  ( -22.90687623753526125, 9.466200233939549236, -230.1557007022273638 ) ) ;
#15938 = CARTESIAN_POINT ( 'NONE',  ( 25.09997929702755926, 1.294103573351435221, -217.0485712200477906 ) ) ;
#15939 = CARTESIAN_POINT ( 'NONE',  ( 6.679827377097204533, -23.59744646493245668, -231.8618301756397670 ) ) ;
#15940 = VERTEX_POINT ( 'NONE', #10578 ) ;
#15941 = CARTESIAN_POINT ( 'NONE',  ( 10.02513374692848913, 18.81568788741115128, -217.1505009242214612 ) ) ;
#15942 = CARTESIAN_POINT ( 'NONE',  ( 20.39962514764921409, -3.647888038500222141, -219.1338420190236036 ) ) ;
#15943 = CARTESIAN_POINT ( 'NONE',  ( 23.12216041205843453, 0.2121350054995089496, -232.0572713672589202 ) ) ;
#15944 = CARTESIAN_POINT ( 'NONE',  ( 8.115778909262310492, -29.92983049028717346, -224.5060555478150377 ) ) ;
#15945 = CARTESIAN_POINT ( 'NONE',  ( -22.99617382825321599, 17.18101613848176967, -230.9512687019100099 ) ) ;
#15947 = CARTESIAN_POINT ( 'NONE',  ( -13.48133478602219171, 10.24771958306113362, -218.3822527490931691 ) ) ;
#15946 = AXIS2_PLACEMENT_3D ( 'NONE', #14999, #21612, #11168 ) ;
#15948 = ORIENTED_EDGE ( 'NONE', *, *, #8288, .F. ) ;
#15949 = CARTESIAN_POINT ( 'NONE',  ( 21.19180206786061405, -1.472355559550188264, -231.3901500139509722 ) ) ;
#15950 = CARTESIAN_POINT ( 'NONE',  ( -24.60063047153272819, -17.11178239752603858, -226.7032704813509554 ) ) ;
#15951 = AXIS2_PLACEMENT_3D ( 'NONE', #19318, #10553, #14051 ) ;
#15952 = DIRECTION ( 'NONE',  ( 0.000000000000000000, 0.000000000000000000, -1.000000000000000000 ) ) ;
#15953 = CARTESIAN_POINT ( 'NONE',  ( 16.07305932912010960, 0.9253679043337685872, -229.0409936706996064 ) ) ;
#15954 = CARTESIAN_POINT ( 'NONE',  ( -12.78558550453068854, 7.693178343823584342, -230.0800953344970878 ) ) ;
#15955 = CARTESIAN_POINT ( 'NONE',  ( 8.168748216644726057, -13.67612414567523693, -220.8005964828080607 ) ) ;
#15956 =( NAMED_UNIT ( * ) SI_UNIT ( $, .STERADIAN. ) SOLID_ANGLE_UNIT ( ) );
#15957 = EDGE_CURVE ( 'NONE', #20136, #2853, #22107, .T. ) ;
#15958 = CARTESIAN_POINT ( 'NONE',  ( 27.66944030902029539, 6.857614156517904291, -220.9860880211026313 ) ) ;
#15959 = CARTESIAN_POINT ( 'NONE',  ( -8.523771322135640816, 24.09653697920728987, -233.1071395647740303 ) ) ;
#15960 = DIRECTION ( 'NONE',  ( 1.000000000000000000, 0.000000000000000000, -0.000000000000000000 ) ) ;
#15961 = CARTESIAN_POINT ( 'NONE',  ( 17.51175949430614409, 14.31829016556564937, -218.8195841045835550 ) ) ;
#15962 = CARTESIAN_POINT ( 'NONE',  ( 4.683166109028750412, -21.42534054955530110, -233.6038185840237986 ) ) ;
#15963 = ORIENTED_EDGE ( 'NONE', *, *, #925, .F. ) ;
#15964 = CARTESIAN_POINT ( 'NONE',  ( 0.3632086708616291126, 21.06287758167331958, -232.5112839711303820 ) ) ;
#15965 = CARTESIAN_POINT ( 'NONE',  ( -12.66290653391502907, 23.44312233264792411, -230.9359094203250606 ) ) ;
#15966 = CARTESIAN_POINT ( 'NONE',  ( -11.78887577478644566, 1.715692547334320084, -224.3106172711415525 ) ) ;
#15967 = CARTESIAN_POINT ( 'NONE',  ( -9.995627826723184839, -14.18420632236771439, -221.4333122433492633 ) ) ;
#15968 = DIRECTION ( 'NONE',  ( 0.000000000000000000, 0.000000000000000000, -1.000000000000000000 ) ) ;
#15969 = AXIS2_PLACEMENT_3D ( 'NONE', #20462, #18686, #1579 ) ;
#15970 = EDGE_LOOP ( 'NONE', ( #19870, #13674 ) ) ;
#15971 = CARTESIAN_POINT ( 'NONE',  ( -26.58771759052039485, 5.114955214121561511, -218.2823714869195442 ) ) ;
#15972 = CARTESIAN_POINT ( 'NONE',  ( 3.112457940538468470, -21.91845672593830940, -231.6743386618371403 ) ) ;
#15973 = CARTESIAN_POINT ( 'NONE',  ( 16.54345861550681107, 19.37554510112122230, -218.2240151908141002 ) ) ;
#15974 = CARTESIAN_POINT ( 'NONE',  ( 4.730976410881341465, 17.65764351829336931, -217.6025626048331674 ) ) ;
#15975 = CARTESIAN_POINT ( 'NONE',  ( -15.72195651633673208, 2.938252489821347346, -222.2698596109374023 ) ) ;
#15976 = CARTESIAN_POINT ( 'NONE',  ( 3.763426558366607111, 28.60172112197566818, -230.1816715025297526 ) ) ;
#15977 = LINE ( 'NONE', #339, #11989 ) ;
#15978 = CARTESIAN_POINT ( 'NONE',  ( -9.078153229956912540, -10.71731945587431056, -228.5228069477245469 ) ) ;
#15979 = CARTESIAN_POINT ( 'NONE',  ( 24.96294718070021901, -13.86220829677249178, -229.4442241490162075 ) ) ;
#15980 = CARTESIAN_POINT ( 'NONE',  ( 0.000000000000000000, 0.000000000000000000, 95.00000000000000000 ) ) ;
#15981 = DIRECTION ( 'NONE',  ( 0.000000000000000000, 0.000000000000000000, -1.000000000000000000 ) ) ;
#15982 = CARTESIAN_POINT ( 'NONE',  ( -9.722597143579921664, 7.159547510896417499, -227.5730737101346222 ) ) ;
#15983 = CARTESIAN_POINT ( 'NONE',  ( -22.11234321210701737, -3.359691084028018526, -230.9311713419302521 ) ) ;
#15984 = CARTESIAN_POINT ( 'NONE',  ( -20.47640197314466093, 18.50423766437512541, -220.4440130802851456 ) ) ;
#15985 = CARTESIAN_POINT ( 'NONE',  ( 15.26539804565921621, 9.309431686815628382, -232.9129599938668207 ) ) ;
#15986 = CARTESIAN_POINT ( 'NONE',  ( -4.211886032913159106, 20.62037006687756602, -216.9488349035050305 ) ) ;
#15987 = ORIENTED_EDGE ( 'NONE', *, *, #70, .T. ) ;
#15988 = CARTESIAN_POINT ( 'NONE',  ( 7.820185266007354308, -13.10000580370673440, -218.6580452893993254 ) ) ;
#15989 = EDGE_LOOP ( 'NONE', ( #11575, #5626, #328, #15586 ) ) ;
#15990 = CARTESIAN_POINT ( 'NONE',  ( 17.34727976380017722, 4.822939981779328811, -230.8836217450937909 ) ) ;
#15991 = EDGE_CURVE ( 'NONE', #10560, #16621, #10616, .T. ) ;
#15992 = CARTESIAN_POINT ( 'NONE',  ( -4.378220565073127624, 31.53459173284372952, -222.0564199190954753 ) ) ;
#15993 = CARTESIAN_POINT ( 'NONE',  ( -4.296082356836364191, 12.57880442405704002, -229.5247240216588125 ) ) ;
#15994 = CARTESIAN_POINT ( 'NONE',  ( -12.22852564478610482, -7.025360622849957437, -222.3415469712626589 ) ) ;
#15995 = CARTESIAN_POINT ( 'NONE',  ( -21.02719846458807851, 18.12262440796364871, -218.0220709499931502 ) ) ;
#15996 = CARTESIAN_POINT ( 'NONE',  ( 0.000000000000000000, 0.000000000000000000, 75.00000000000000000 ) ) ;
#15997 = CARTESIAN_POINT ( 'NONE',  ( 15.13105790938820228, -1.902449014147146178, -222.1588331224812407 ) ) ;
#15998 = CIRCLE ( 'NONE', #6279, 3.000000000000002665 ) ;
#15999 = CARTESIAN_POINT ( 'NONE',  ( -12.15411956849120756, 11.21601165624538687, -228.1895064089065670 ) ) ;
#16000 = COLOUR_RGB ( '', 0.08235294, 0.09019608, 0.10196078) ;
#16001 = CARTESIAN_POINT ( 'NONE',  ( 20.09685469220202236, -2.033783885649083079, -233.1448060988079760 ) ) ;
#16002 = CARTESIAN_POINT ( 'NONE',  ( -13.69675006931110417, 3.702342960760605539, -228.0723273272095355 ) ) ;
#16003 = CARTESIAN_POINT ( 'NONE',  ( 11.67669251569587985, 24.04736029062789981, -218.5856804285192254 ) ) ;
#16004 = CARTESIAN_POINT ( 'NONE',  ( -14.33274213004767716, -3.240524307521291725, -229.5155949954044559 ) ) ;
#16005 = CARTESIAN_POINT ( 'NONE',  ( 1.719513778997906694, 15.52930330544231730, -222.3959083836286368 ) ) ;
#16006 = CARTESIAN_POINT ( 'NONE',  ( -5.902479482706956659, -14.78727544128710214, -218.5565286504736946 ) ) ;
#16007 = CARTESIAN_POINT ( 'NONE',  ( 5.248230734842167955, 23.54336384919183445, -216.8914391693808739 ) ) ;
#16008 = CARTESIAN_POINT ( 'NONE',  ( 15.50373320885645079, -27.90820408561472732, -228.0623419774833280 ) ) ;
#16009 = CARTESIAN_POINT ( 'NONE',  ( -24.25245498015852874, 0.2109992039763788352, -218.1398602137601301 ) ) ;
#16010 = CARTESIAN_POINT ( 'NONE',  ( -11.05032764129755840, 11.65053160594169945, -221.1796278216217218 ) ) ;
#16011 =( LENGTH_UNIT ( ) NAMED_UNIT ( * ) SI_UNIT ( .MILLI., .METRE. ) );
#16012 = CARTESIAN_POINT ( 'NONE',  ( 20.28526114930425450, -5.837089636085359245, -233.7994602772149051 ) ) ;
#16013 = CARTESIAN_POINT ( 'NONE',  ( 9.253909228257674258, 17.69332415812615977, -230.9900471521432621 ) ) ;
#16014 = CARTESIAN_POINT ( 'NONE',  ( -14.57944476639264764, 6.129437248167259433, -229.4766146696829310 ) ) ;
#16015 = CARTESIAN_POINT ( 'NONE',  ( 15.52719855059926424, 1.633696074270991172, -221.7349885876216433 ) ) ;
#16016 = CARTESIAN_POINT ( 'NONE',  ( -7.732225105831920686, -12.76821222370703346, -228.2562058524068220 ) ) ;
#16017 = AXIS2_PLACEMENT_3D ( 'NONE', #5055, #11931, #18798 ) ;
#16018 = AXIS2_PLACEMENT_3D ( 'NONE', #10968, #8955, #15819 ) ;
#16019 = CARTESIAN_POINT ( 'NONE',  ( 8.681721411120292942, 8.442847255497570202, -228.0516816418615065 ) ) ;
#16020 = DIRECTION ( 'NONE',  ( 1.000000000000000000, 0.000000000000000000, 0.000000000000000000 ) ) ;
#16021 = CARTESIAN_POINT ( 'NONE',  ( -4.907461209876205821, -14.28794023480369368, -232.2749568027591636 ) ) ;
#16022 = CARTESIAN_POINT ( 'NONE',  ( 3.080453011304693511, 29.32691491905673331, -222.8956499783474499 ) ) ;
#16023 = CARTESIAN_POINT ( 'NONE',  ( 8.379126514044342500, 15.76264856365358646, -232.1787896114811360 ) ) ;
#16024 = CARTESIAN_POINT ( 'NONE',  ( -17.99155049254074612, 5.190958499132906745, -220.1449419322306937 ) ) ;
#16025 = ADVANCED_FACE ( 'NONE', ( #14076 ), #9005, .T. ) ;
#16026 = CARTESIAN_POINT ( 'NONE',  ( -5.340143745732740754, 22.10628181454592678, -235.0476201740528097 ) ) ;
#16027 = CARTESIAN_POINT ( 'NONE',  ( 14.92135368508905202, 7.451356898669101447, -219.1823315336843621 ) ) ;
#16028 = ORIENTED_EDGE ( 'NONE', *, *, #10351, .F. ) ;
#16029 = CARTESIAN_POINT ( 'NONE',  ( 18.69764316139794147, -20.69319383826335823, -224.5905439953889413 ) ) ;
#16030 = EDGE_LOOP ( 'NONE', ( #11090, #7413, #7481, #4790 ) ) ;
#16031 = CARTESIAN_POINT ( 'NONE',  ( 8.158223302632384488, -13.44420475212243993, -229.3230086144918403 ) ) ;
#16032 = EDGE_CURVE ( 'NONE', #18699, #18628, #14571, .T. ) ;
#16033 = CARTESIAN_POINT ( 'NONE',  ( -8.115738378024497379, 16.90402287339461296, -219.0833473190803034 ) ) ;
#16034 = ORIENTED_EDGE ( 'NONE', *, *, #22184, .F. ) ;
#16035 = DIRECTION ( 'NONE',  ( 0.000000000000000000, -0.7999999999999999334, -0.6000000000000000888 ) ) ;
#16036 = CARTESIAN_POINT ( 'NONE',  ( 14.95414693437772868, 8.262206471704862665, -230.1862972580043163 ) ) ;
#16037 = CARTESIAN_POINT ( 'NONE',  ( -20.69232116990083981, -0.6602618815637216754, -233.8806059993499957 ) ) ;
#16038 = CARTESIAN_POINT ( 'NONE',  ( -13.22951852716680676, -5.246159916193459338, -223.7538483380451453 ) ) ;
#16039 = CARTESIAN_POINT ( 'NONE',  ( 1.799766247726228174, -14.75051420185460849, -230.6199496058247291 ) ) ;
#16040 = CARTESIAN_POINT ( 'NONE',  ( 3.241594727517011609, 27.64703009302456138, -225.5540025036233374 ) ) ;
#16041 = DIRECTION ( 'NONE',  ( -1.000000000000000000, 0.000000000000000000, 0.000000000000000000 ) ) ;
#16042 = CARTESIAN_POINT ( 'NONE',  ( -20.49711526797010208, 7.006997077916217620, -215.3369776077118445 ) ) ;
#16043 = CARTESIAN_POINT ( 'NONE',  ( -4.620781219515533778, 16.99182040716223696, -217.1278208835672672 ) ) ;
#16044 = CARTESIAN_POINT ( 'NONE',  ( 3.388180927852674884, 15.71154068801650538, -224.9339660840813053 ) ) ;
#16045 = VERTEX_POINT ( 'NONE', #21463 ) ;
#16046 = CARTESIAN_POINT ( 'NONE',  ( -1.975202609796049336, 20.81351768191813889, -217.5779402428482001 ) ) ;
#16047 = CARTESIAN_POINT ( 'NONE',  ( -22.10934047915413814, 0.9940043559354462266, -218.9999999999999716 ) ) ;
#16048 = CARTESIAN_POINT ( 'NONE',  ( 16.22460398937575121, -0.7285105026664867589, -219.3274985887512116 ) ) ;
#16049 = CARTESIAN_POINT ( 'NONE',  ( 13.65368867897269389, -25.84127502057983605, -227.3223880387346867 ) ) ;
#16051 = CARTESIAN_POINT ( 'NONE',  ( -21.00000000000000000, 0.000000000000000000, -75.00000000000000000 ) ) ;
#16050 = AXIS2_PLACEMENT_3D ( 'NONE', #2319, #9205, #21216 ) ;
#16052 = CARTESIAN_POINT ( 'NONE',  ( 21.96352831578809273, -0.3315607655629317918, -233.9427286327412503 ) ) ;
#16053 = CARTESIAN_POINT ( 'NONE',  ( 12.53674998645855787, 17.96979015029927851, -232.8843215672231679 ) ) ;
#16054 = CARTESIAN_POINT ( 'NONE',  ( 15.67226265972355392, -3.922905252720024105, -226.2579514984929858 ) ) ;
#16055 = CARTESIAN_POINT ( 'NONE',  ( 26.16486877413895584, -0.2437668799822691745, -230.8325409000573814 ) ) ;
#16056 = EDGE_CURVE ( 'NONE', #7254, #20783, #16714, .T. ) ;
#16057 = CARTESIAN_POINT ( 'NONE',  ( 4.682724365302521896, -22.35092628325669750, -215.9543778044225348 ) ) ;
#16058 = APPLICATION_CONTEXT ( 'automotive_design' ) ;
#16059 = APPLICATION_PROTOCOL_DEFINITION ( 'draft international standard', 'automotive_design', 1998, #16058 ) ;
#16060 = CARTESIAN_POINT ( 'NONE',  ( -23.52999999174766543, 19.39566142560855866, -221.9446938626390704 ) ) ;
#16061 = CARTESIAN_POINT ( 'NONE',  ( -19.90771709537278156, 23.83218599423810602, -225.0439263757368735 ) ) ;
#16062 = EDGE_LOOP ( 'NONE', ( #10318, #7508, #13138, #8772, #19620, #5674 ) ) ;
#16063 = CARTESIAN_POINT ( 'NONE',  ( -23.98802705797876200, 19.46654170242919690, -223.5293093576406989 ) ) ;
#16064 = CARTESIAN_POINT ( 'NONE',  ( -17.90134810484358141, -14.13951559615540710, -232.9640066987647344 ) ) ;
#16065 = CARTESIAN_POINT ( 'NONE',  ( 0.000000000000000000, 0.000000000000000000, -25.00000000000000000 ) ) ;
#16066 = CARTESIAN_POINT ( 'NONE',  ( -9.151299407007059017, 9.196974979111923076, -223.9483834032048719 ) ) ;
#16067 = CARTESIAN_POINT ( 'NONE',  ( 3.692943796146577196, -17.43777048755501724, -232.3481250940208156 ) ) ;
#16068 = LINE ( 'NONE', #14382, #8131 ) ;
#16069 = CARTESIAN_POINT ( 'NONE',  ( -11.98736441306973077, 11.45674391201457176, -217.8252237716743025 ) ) ;
#16070 = CARTESIAN_POINT ( 'NONE',  ( 19.31922195716811430, 9.600631919686000160, -218.1359845693048101 ) ) ;
#16071 = CARTESIAN_POINT ( 'NONE',  ( -11.87391433320165746, 8.920676825367966245, -232.2044275666449096 ) ) ;
#16072 = DIRECTION ( 'NONE',  ( -0.000000000000000000, -0.000000000000000000, 1.000000000000000000 ) ) ;
#16073 = CARTESIAN_POINT ( 'NONE',  ( -16.40095417437164471, 2.582410108382750646, -233.5151473761628154 ) ) ;
#16074 = CARTESIAN_POINT ( 'NONE',  ( -10.27880337231260199, -13.06498408352235430, -227.3766186522184682 ) ) ;
#16075 = EDGE_LOOP ( 'NONE', ( #16034, #13421, #12389, #12877 ) ) ;
#16076 = CARTESIAN_POINT ( 'NONE',  ( -9.810154340578240095, 25.84808829058669488, -220.5759521898573610 ) ) ;
#16077 = EDGE_CURVE ( 'NONE', #17072, #16801, #11132, .T. ) ;
#16078 = CARTESIAN_POINT ( 'NONE',  ( -17.07311071032027172, 18.59516984069744794, -230.9440421721702137 ) ) ;
#16079 = CARTESIAN_POINT ( 'NONE',  ( -12.27164519775873686, 10.97713184439464840, -231.6269036897678291 ) ) ;
#16080 = CARTESIAN_POINT ( 'NONE',  ( -9.780669591740702273, -13.62818526938769104, -222.3368934028275135 ) ) ;
#16081 = FACE_OUTER_BOUND ( 'NONE', #10856, .T. ) ;
#16082 = ORIENTED_EDGE ( 'NONE', *, *, #9403, .F. ) ;
#16083 = CARTESIAN_POINT ( 'NONE',  ( 16.40130693394614525, -0.1574073183566240264, -221.9481963320051534 ) ) ;
#16084 = CARTESIAN_POINT ( 'NONE',  ( 0.6118723529980315545, -20.11903950562274446, -217.9558718073025716 ) ) ;
#16085 = CARTESIAN_POINT ( 'NONE',  ( 22.86997486125673618, 17.56009411325475966, -222.3578648042903296 ) ) ;
#16086 = CARTESIAN_POINT ( 'NONE',  ( 5.017623471397871349, 29.83561274492976878, -222.9769172135417250 ) ) ;
#16087 = CARTESIAN_POINT ( 'NONE',  ( -25.11055959288653128, 8.701823109978603199, -230.2231080656787583 ) ) ;
#16088 = CARTESIAN_POINT ( 'NONE',  ( 12.99334571784053338, 27.47142594410712846, -219.5003755906066658 ) ) ;
#16089 = CARTESIAN_POINT ( 'NONE',  ( 15.33737796850231305, 13.57479350230705428, -232.3313557812109025 ) ) ;
#16090 = CARTESIAN_POINT ( 'NONE',  ( 14.58114346306845377, 2.033664520579581581, -222.7937709467664149 ) ) ;
#16091 = CARTESIAN_POINT ( 'NONE',  ( -5.525229149912007642, -13.32411127922494742, -220.4018445532201440 ) ) ;
#16092 = CARTESIAN_POINT ( 'NONE',  ( 4.201723131641114328, -20.76291977712905279, -215.9522215885928347 ) ) ;
#16093 = CARTESIAN_POINT ( 'NONE',  ( 1.526556658859590496E-13, -21.00000000000006040, -69.99999999999998579 ) ) ;
#16094 = LINE ( 'NONE', #12930, #14122 ) ;
#16095 = CARTESIAN_POINT ( 'NONE',  ( -16.95112677453439431, 10.32962960657076934, -214.9445123409346650 ) ) ;
#16096 = CARTESIAN_POINT ( 'NONE',  ( -18.83136555461844708, -9.493528738360442532, -219.1308048892593945 ) ) ;
#16097 = CARTESIAN_POINT ( 'NONE',  ( -15.82622499106666325, 9.895986579907866343, -218.5115209877527604 ) ) ;
#16098 = CARTESIAN_POINT ( 'NONE',  ( 9.798337081649805214, 12.27506320122302697, -218.9346733583377613 ) ) ;
#16099 = CARTESIAN_POINT ( 'NONE',  ( 7.951191770265756631, 20.55701948568933091, -231.2149185317973661 ) ) ;
#16100 = ORIENTED_EDGE ( 'NONE', *, *, #11353, .T. ) ;
#16101 = CARTESIAN_POINT ( 'NONE',  ( 19.66172111867919270, -11.21951684559458506, -235.3531537740016972 ) ) ;
#16102 = CARTESIAN_POINT ( 'NONE',  ( 14.54149994592679107, 8.070685273005897997, -229.7292930672863349 ) ) ;
#16103 = CARTESIAN_POINT ( 'NONE',  ( -11.59874896804548250, 27.28969409813203484, -218.8626241359735332 ) ) ;
#16104 = CARTESIAN_POINT ( 'NONE',  ( -12.39195900010699702, 23.13258866008456138, -233.4668451572263166 ) ) ;
#16105 = CARTESIAN_POINT ( 'NONE',  ( -17.60306105620566441, -10.62493847279374926, -216.8163279515337649 ) ) ;
#16106 = CARTESIAN_POINT ( 'NONE',  ( -11.49049084071896409, 11.06834963248926940, -218.3354249205727058 ) ) ;
#16107 = CARTESIAN_POINT ( 'NONE',  ( -10.55583158923998077, -9.946257437971063098, 93.00000000000002842 ) ) ;
#16108 = CARTESIAN_POINT ( 'NONE',  ( 20.15756451863428111, -2.090604891399794774, -217.8900786001194945 ) ) ;
#16109 = CARTESIAN_POINT ( 'NONE',  ( 1.773237071419721422, 13.09828209437875302, -220.6531024550077404 ) ) ;
#16110 = CARTESIAN_POINT ( 'NONE',  ( -21.89065952084834166, -0.9940043559354216907, -218.9999999999999716 ) ) ;
#16111 = CARTESIAN_POINT ( 'NONE',  ( -25.80904414196669450, 12.19501778665756220, -219.1732313092283846 ) ) ;
#16112 = CARTESIAN_POINT ( 'NONE',  ( 4.559463107227270662, 13.27337529356814017, -226.9596205199204633 ) ) ;
#16113 = PLANE ( 'NONE',  #7642 ) ;
#16114 = CARTESIAN_POINT ( 'NONE',  ( -1.248802714212398968, 14.93471382136348602, -228.4293827518713158 ) ) ;
#16115 = CARTESIAN_POINT ( 'NONE',  ( -15.19144047750087267, -10.24270553329939304, -232.4311702607364793 ) ) ;
#16116 = CARTESIAN_POINT ( 'NONE',  ( 11.82943521288609823, 27.58963564415041247, -226.1180395413371400 ) ) ;
#16117 = CARTESIAN_POINT ( 'NONE',  ( 20.49803729918260942, -22.47924998572259980, -218.9346008044765028 ) ) ;
#16118 = LINE ( 'NONE', #11160, #7427 ) ;
#16119 = CARTESIAN_POINT ( 'NONE',  ( -13.93825237094548619, 9.044872709574327985, -220.1275804576921757 ) ) ;
#16120 = CARTESIAN_POINT ( 'NONE',  ( 12.94117841657163126, -3.283311917827119064, -226.8844617769393039 ) ) ;
#16121 = CARTESIAN_POINT ( 'NONE',  ( 14.96080648943632241, 22.28365808184747721, -220.1237743409445216 ) ) ;
#16122 = CARTESIAN_POINT ( 'NONE',  ( -19.74163224554151697, 8.726897413558679872, -232.6665747339030190 ) ) ;
#16124 = CIRCLE ( 'NONE', #22235, 23.00000000000008882 ) ;
#16123 = CARTESIAN_POINT ( 'NONE',  ( 28.57344184061583192, 5.631897254180425527, -225.1192013637692355 ) ) ;
#16125 = CARTESIAN_POINT ( 'NONE',  ( -15.97267037792306255, -23.58045393237649279, -221.6247985403941527 ) ) ;
#16126 = CARTESIAN_POINT ( 'NONE',  ( 21.77779027533950540, 18.43917590911969029, -232.9503911151153659 ) ) ;
#16127 = DIRECTION ( 'NONE',  ( -1.000000000000000000, 0.000000000000000000, 0.000000000000000000 ) ) ;
#16128 = CARTESIAN_POINT ( 'NONE',  ( -27.27535713358387781, -16.47971293676793181, -227.4585470903502653 ) ) ;
#16129 = CARTESIAN_POINT ( 'NONE',  ( 1.104227501629593045, 25.05528885094460989, -231.9808705443460326 ) ) ;
#16130 = CARTESIAN_POINT ( 'NONE',  ( 15.96089671440110713, 1.143943728337336374, -218.3532651118343892 ) ) ;
#16131 = CARTESIAN_POINT ( 'NONE',  ( -9.969679877803788060, 12.84542071557917176, -220.4758784541224657 ) ) ;
#16132 = AXIS2_PLACEMENT_3D ( 'NONE', #217, #17436, #7086 ) ;
#16133 = CARTESIAN_POINT ( 'NONE',  ( -8.123851230256436295, 20.56863949923577550, -215.0796075421103239 ) ) ;
#16134 = CARTESIAN_POINT ( 'NONE',  ( -18.71530386740073126, -0.6857509888707814527, -217.6195632122020527 ) ) ;
#16135 = EDGE_CURVE ( 'NONE', #7787, #15223, #192, .T. ) ;
#16136 = CARTESIAN_POINT ( 'NONE',  ( -2.392195434554431177, -23.29395655963766387, -232.4094703796048691 ) ) ;
#16137 = ORIENTED_EDGE ( 'NONE', *, *, #19244, .T. ) ;
#16138 = CARTESIAN_POINT ( 'NONE',  ( 8.339826811406878093, -13.81198187275966660, -229.8741491687588621 ) ) ;
#16139 = CYLINDRICAL_SURFACE ( 'NONE', #13841, 2.000000000000000000 ) ;
#16140 = CARTESIAN_POINT ( 'NONE',  ( 15.61962121506769385, 4.525360868525488911, -229.0684696061408090 ) ) ;
#16141 = CARTESIAN_POINT ( 'NONE',  ( -13.00301829581513857, -0.4478114825397079279, -224.9470972339195214 ) ) ;
#16142 = CARTESIAN_POINT ( 'NONE',  ( -18.53787071664277519, -6.556543064843903146, -232.5192140591401824 ) ) ;
#16143 = CARTESIAN_POINT ( 'NONE',  ( 8.532614294830283441, -28.73326933124977955, -229.1610356131385231 ) ) ;
#16144 = CARTESIAN_POINT ( 'NONE',  ( 3.433394806375676733, 19.92272173529517332, -219.3341428536850799 ) ) ;
#16145 = DIRECTION ( 'NONE',  ( 0.000000000000000000, -1.000000000000000000, 0.000000000000000000 ) ) ;
#16146 = CARTESIAN_POINT ( 'NONE',  ( -29.50764134580612463, 7.783340782857166573, -219.9768238800827191 ) ) ;
#16147 = CARTESIAN_POINT ( 'NONE',  ( -8.966714183099560032, 19.05224306381768073, -234.0879867025980445 ) ) ;
#16148 = CARTESIAN_POINT ( 'NONE',  ( 3.433394806375676733, 19.92272173529517332, -219.3341428536850799 ) ) ;
#16149 = CARTESIAN_POINT ( 'NONE',  ( 12.70896864779121316, -3.955665148817821386, -221.1719243096075900 ) ) ;
#16150 = ORIENTED_EDGE ( 'NONE', *, *, #5782, .T. ) ;
#16151 = ORIENTED_EDGE ( 'NONE', *, *, #17798, .F. ) ;
#16152 = CARTESIAN_POINT ( 'NONE',  ( 9.211411085256067111, 16.86455563410128633, -232.8411836211112700 ) ) ;
#16153 = CARTESIAN_POINT ( 'NONE',  ( -18.02718827071834085, 20.33515877052379395, -229.5060669840136143 ) ) ;
#16154 = CARTESIAN_POINT ( 'NONE',  ( 17.72360441613731652, -1.822637811265336749, -232.2813868768326984 ) ) ;
#16155 = ADVANCED_FACE ( 'NONE', ( #12711 ), #3043, .F. ) ;
#16156 = CARTESIAN_POINT ( 'NONE',  ( -5.218961787268129093, -16.18493974670746027, -219.8229902141834771 ) ) ;
#16157 = CARTESIAN_POINT ( 'NONE',  ( 0.000000000000000000, 0.000000000000000000, -24.99999999999999645 ) ) ;
#16158 = CARTESIAN_POINT ( 'NONE',  ( -21.63401512838747820, 0.000000000000000000, -77.51594804401857175 ) ) ;
#16159 = CARTESIAN_POINT ( 'NONE',  ( 8.979547488457603421, 23.24376652602565230, -232.6628827740196357 ) ) ;
#16160 = CARTESIAN_POINT ( 'NONE',  ( 13.39501375133567329, -10.34300172232987691, -228.1452887455185987 ) ) ;
#16161 = PLANE ( 'NONE',  #10815 ) ;
#16162 = CARTESIAN_POINT ( 'NONE',  ( 6.260999666360449467, -13.19315344885661645, -220.2890618333529744 ) ) ;
#16163 = CONTEXT_DEPENDENT_SHAPE_REPRESENTATION ( #21353, #1502 ) ;
#16164 = CARTESIAN_POINT ( 'NONE',  ( 3.449504654906655254, 27.59247159270940841, -231.3461799890608859 ) ) ;
#16165 = CARTESIAN_POINT ( 'NONE',  ( -23.89856910807799295, 17.42297078648622843, -222.0178620725767757 ) ) ;
#16166 = ORIENTED_EDGE ( 'NONE', *, *, #12459, .F. ) ;
#16167 = CARTESIAN_POINT ( 'NONE',  ( -13.83274569775339202, 16.20364235096346661, -234.0851861771356539 ) ) ;
#16168 = CARTESIAN_POINT ( 'NONE',  ( -17.81508947870519322, -18.77243306401324219, -218.1930932538018340 ) ) ;
#16169 = FACE_OUTER_BOUND ( 'NONE', #16614, .T. ) ;
#16170 = DIRECTION ( 'NONE',  ( 0.000000000000000000, 0.000000000000000000, -1.000000000000000000 ) ) ;
#16171 = CARTESIAN_POINT ( 'NONE',  ( -7.189383125363055349, 14.28512618638020548, -231.7475838278701303 ) ) ;
#16172 = CARTESIAN_POINT ( 'NONE',  ( 8.625046000483031605, -27.40455649025574303, -220.2318935480384710 ) ) ;
#16173 = CARTESIAN_POINT ( 'NONE',  ( 21.63401512838757768, 0.000000000000000000, 77.51594804401857175 ) ) ;
#16174 = CARTESIAN_POINT ( 'NONE',  ( -23.98802705797876200, 19.46654170242919690, -223.5293093576406989 ) ) ;
#16175 = CARTESIAN_POINT ( 'NONE',  ( -22.28357709049062407, 7.264818440526320309, -215.3877468064711707 ) ) ;
#16176 = CARTESIAN_POINT ( 'NONE',  ( -1.238249567024760189, 29.30580384236933966, -223.2399636023643836 ) ) ;
#16177 = CARTESIAN_POINT ( 'NONE',  ( 0.000000000000000000, 0.000000000000000000, -126.0000000000000284 ) ) ;
#16178 = CARTESIAN_POINT ( 'NONE',  ( 14.68130101653174613, 6.427210486143660084, -228.0153742661088074 ) ) ;
#16179 = CARTESIAN_POINT ( 'NONE',  ( -10.61621529918308227, -15.65610094335291969, -220.0975530242428420 ) ) ;
#16180 = VERTEX_POINT ( 'NONE', #19999 ) ;
#16181 = CARTESIAN_POINT ( 'NONE',  ( 9.211411085256067111, 16.86455563410128633, -232.8411836211112700 ) ) ;
#16182 = CARTESIAN_POINT ( 'NONE',  ( -12.69709334397052203, 10.59859500067950400, -221.6107941937004568 ) ) ;
#16183 = CARTESIAN_POINT ( 'NONE',  ( -13.71158422780231056, 12.21432067443984693, -232.9166272955793033 ) ) ;
#16184 = CARTESIAN_POINT ( 'NONE',  ( -18.52912398332900068, -6.554396152115366192, -218.2980051671528088 ) ) ;
#16185 = FACE_OUTER_BOUND ( 'NONE', #4928, .T. ) ;
#16186 = ORIENTED_EDGE ( 'NONE', *, *, #1896, .F. ) ;
#16187 = CARTESIAN_POINT ( 'NONE',  ( -15.15434969228324924, 4.423874646950748613, -230.6144467931089821 ) ) ;
#16188 = CARTESIAN_POINT ( 'NONE',  ( 4.239709385547987708, -16.34504625405869405, -220.9645569933060756 ) ) ;
#16189 = CARTESIAN_POINT ( 'NONE',  ( 15.57223476564572984, 1.638033498045565306, -221.8258985305325268 ) ) ;
#16190 = CARTESIAN_POINT ( 'NONE',  ( 3.449504654906655254, 27.59247159270940841, -231.3461799890608859 ) ) ;
#16191 = CARTESIAN_POINT ( 'NONE',  ( 0.000000000000000000, 19.80000000000006111, -78.50000000000000000 ) ) ;
#16192 = CARTESIAN_POINT ( 'NONE',  ( -22.14646582578067679, 6.967411055428133437, -231.6932229095398270 ) ) ;
#16193 = CARTESIAN_POINT ( 'NONE',  ( 16.71272566993619080, 8.989703107375911273, -217.4612081447889125 ) ) ;
#16194 = CARTESIAN_POINT ( 'NONE',  ( 10.78187269046063435, 10.73871010366167944, -221.9206544238666368 ) ) ;
#16195 = DIRECTION ( 'NONE',  ( 0.000000000000000000, 0.000000000000000000, -1.000000000000000000 ) ) ;
#16196 = CARTESIAN_POINT ( 'NONE',  ( -5.636842872076440081, -13.76003991320737541, -219.7405193562604495 ) ) ;
#16197 = CARTESIAN_POINT ( 'NONE',  ( 1.799766247726228174, -14.75051420185460849, -230.6199496058247291 ) ) ;
#16198 = CARTESIAN_POINT ( 'NONE',  ( -21.81074228087361178, -7.304017576129684386, -6.837760653483515583 ) ) ;
#16199 = DIRECTION ( 'NONE',  ( -1.000000000000000000, 0.000000000000000000, 0.000000000000000000 ) ) ;
#16200 = CARTESIAN_POINT ( 'NONE',  ( -5.607934827417612844, 15.68271927908880770, -232.1026723719274969 ) ) ;
#16201 = CARTESIAN_POINT ( 'NONE',  ( 20.57969228301723419, -8.207465571703625784, -214.6085555290863454 ) ) ;
#16202 = CARTESIAN_POINT ( 'NONE',  ( 24.56541673123750158, -5.996287403333383281, -231.6940117905984664 ) ) ;
#16203 = CARTESIAN_POINT ( 'NONE',  ( 12.74913679152205148, 9.185760885856177893, -218.6542381594888980 ) ) ;
#16204 = CARTESIAN_POINT ( 'NONE',  ( 8.539351012053531420, 16.03230746435535181, -220.6282946404833751 ) ) ;
#16205 = ADVANCED_FACE ( 'NONE', ( #9448 ), #15646, .T. ) ;
#16206 = ORIENTED_EDGE ( 'NONE', *, *, #7776, .T. ) ;
#16207 = CARTESIAN_POINT ( 'NONE',  ( 20.77649313750695370, -15.65279155457156435, -215.5859610257211898 ) ) ;
#16208 = CARTESIAN_POINT ( 'NONE',  ( 8.814245471595175019, 11.67815946035151953, 93.00000000000000000 ) ) ;
#16209 = CARTESIAN_POINT ( 'NONE',  ( 4.065638640983322283, 32.08830473489500434, -226.0249194102539150 ) ) ;
#16210 = CARTESIAN_POINT ( 'NONE',  ( -5.373457274256926652, 30.83572167890261184, -229.2199105909169532 ) ) ;
#16211 = CARTESIAN_POINT ( 'NONE',  ( -19.98462433625633494, -12.30084073857678639, -216.8518508258974862 ) ) ;
#16212 = CARTESIAN_POINT ( 'NONE',  ( -22.99617382825321599, 17.18101613848176967, -230.9512687019100099 ) ) ;
#16213 = DIRECTION ( 'NONE',  ( 1.000000000000000000, 0.000000000000000000, 0.000000000000000000 ) ) ;
#16214 = CARTESIAN_POINT ( 'NONE',  ( 20.89700225552940793, -4.547446057044195911, -232.3806459760843666 ) ) ;
#16215 = CARTESIAN_POINT ( 'NONE',  ( 2.892356176081334773, 24.03953794589038395, -215.3901262983647200 ) ) ;
#16216 = CARTESIAN_POINT ( 'NONE',  ( 16.67941620816951698, 4.093285459228785506, -217.1675623234529269 ) ) ;
#16217 = CARTESIAN_POINT ( 'NONE',  ( -9.443239614166923701, 9.388015667058336788, -222.3195230688234290 ) ) ;
#16218 = CARTESIAN_POINT ( 'NONE',  ( 20.41153371889344825, 17.18812948447019551, -230.7531656956970778 ) ) ;
#16219 = LINE ( 'NONE', #14755, #9805 ) ;
#16220 = CARTESIAN_POINT ( 'NONE',  ( 5.104697752190542559, 17.18208638613223016, -220.3923334988619445 ) ) ;
#16221 = CARTESIAN_POINT ( 'NONE',  ( -12.04756914620937636, -13.80987496524771885, -232.8991007102355582 ) ) ;
#16222 = CARTESIAN_POINT ( 'NONE',  ( 13.03557269046774714, 7.519834803053426775, -226.9490612297269081 ) ) ;
#16223 = CARTESIAN_POINT ( 'NONE',  ( -2.619247311076123630, -29.90652300472198988, -220.3405913430138128 ) ) ;
#16224 = CARTESIAN_POINT ( 'NONE',  ( 21.82657638218438478, 0.1729100361068894309, -222.0037591556030918 ) ) ;
#16225 = CARTESIAN_POINT ( 'NONE',  ( -16.28025842329327944, 6.985656672962045732, -231.4191468057695715 ) ) ;
#16226 = DIRECTION ( 'NONE',  ( 0.000000000000000000, 0.000000000000000000, 1.000000000000000000 ) ) ;
#16227 = CARTESIAN_POINT ( 'NONE',  ( -29.37537067777813604, -4.151788015186005154, -225.5750753894876368 ) ) ;
#16228 = CARTESIAN_POINT ( 'NONE',  ( 3.174664235197445006, 17.30896320251298448, -221.0803896709622620 ) ) ;
#16229 = CARTESIAN_POINT ( 'NONE',  ( -11.05032764129755840, 11.65053160594169945, -221.1796278216217218 ) ) ;
#16230 = CARTESIAN_POINT ( 'NONE',  ( -14.63872435137796302, 9.306825831109410530, -216.0000338566471214 ) ) ;
#16231 = CARTESIAN_POINT ( 'NONE',  ( -7.928105003701093167, -26.09134507487772225, -231.8683635223868578 ) ) ;
#16232 = CARTESIAN_POINT ( 'NONE',  ( 13.12946830070648652, 6.370976456471619365, -231.5124810213676483 ) ) ;
#16233 = LINE ( 'NONE', #10731, #18077 ) ;
#16234 = CARTESIAN_POINT ( 'NONE',  ( -13.68978490692228256, -5.239663260684684687, -218.7416303080107411 ) ) ;
#16235 = CARTESIAN_POINT ( 'NONE',  ( -3.223980134944351317, 26.83284996841001302, -219.5167893230652965 ) ) ;
#16236 = CARTESIAN_POINT ( 'NONE',  ( 21.72366288329714834, 2.385777479048636351, -215.9150265590827757 ) ) ;
#16237 = CARTESIAN_POINT ( 'NONE',  ( -7.266348978356541366, 16.38312187400933340, -217.9429203627011873 ) ) ;
#16238 = CARTESIAN_POINT ( 'NONE',  ( 3.764125772070460396, 11.78312483992801596, -228.3484643988637970 ) ) ;
#16239 = ORIENTED_EDGE ( 'NONE', *, *, #3764, .T. ) ;
#16240 = CARTESIAN_POINT ( 'NONE',  ( 1.312189596842585404, -27.84482500255423432, -221.0181370286903473 ) ) ;
#16241 = ORIENTED_EDGE ( 'NONE', *, *, #2466, .T. ) ;
#16242 = CARTESIAN_POINT ( 'NONE',  ( -1.615718423935818437, -15.01490656935555812, -223.2481059054151729 ) ) ;
#16243 = DIRECTION ( 'NONE',  ( 0.000000000000000000, -0.6000000000000000888, 0.7999999999999999334 ) ) ;
#16244 = AXIS2_PLACEMENT_3D ( 'NONE', #5290, #4875, #3603 ) ;
#16245 = CARTESIAN_POINT ( 'NONE',  ( 14.63113973005795643, 4.926264598692385199, -222.4866305912601945 ) ) ;
#16246 = CARTESIAN_POINT ( 'NONE',  ( 14.18709644517307922, -11.45356969546147496, -232.2178450427173004 ) ) ;
#16247 = CARTESIAN_POINT ( 'NONE',  ( -12.14186164972853810, -9.217338937739926408, -220.4665480714278374 ) ) ;
#16248 = CARTESIAN_POINT ( 'NONE',  ( -16.75313578746775889, -14.38352658620038937, -216.6304878158699978 ) ) ;
#16249 = CARTESIAN_POINT ( 'NONE',  ( 4.555016420009541989, 17.65848956729471197, -229.5875910199184204 ) ) ;
#16250 = FACE_OUTER_BOUND ( 'NONE', #12485, .T. ) ;
#16251 = CARTESIAN_POINT ( 'NONE',  ( -19.26845014167239611, 9.481468541508135672, -234.4856117705182328 ) ) ;
#16252 = CARTESIAN_POINT ( 'NONE',  ( 4.730976410881341465, 17.65764351829336931, -217.6025626048331674 ) ) ;
#16253 = CARTESIAN_POINT ( 'NONE',  ( -2.543684969149407227, 16.28137730373167713, -227.6987697727321915 ) ) ;
#16254 = CARTESIAN_POINT ( 'NONE',  ( 15.24707275637840453, -5.950922448839978784, -232.7034617680506869 ) ) ;
#16255 = EDGE_LOOP ( 'NONE', ( #17230, #6482 ) ) ;
#16256 = CARTESIAN_POINT ( 'NONE',  ( 8.903385417657583289, 10.41040586594612272, -227.6527940987422198 ) ) ;
#16257 = CARTESIAN_POINT ( 'NONE',  ( -25.20870746202117729, 11.68425842440532136, -223.9066764530103342 ) ) ;
#16258 = CARTESIAN_POINT ( 'NONE',  ( 14.29548763234129538, 2.320071712424730315, -230.2610858871018422 ) ) ;
#16259 = CARTESIAN_POINT ( 'NONE',  ( -6.723652888800149441, -28.28510889945508211, -226.1741921951756638 ) ) ;
#16260 = PLANE ( 'NONE',  #5804 ) ;
#16261 = CARTESIAN_POINT ( 'NONE',  ( 0.000000000000000000, 0.000000000000000000, -75.00000000000000000 ) ) ;
#16262 = EDGE_CURVE ( 'NONE', #10887, #580, #14409, .T. ) ;
#16263 = AXIS2_PLACEMENT_3D ( 'NONE', #5970, #6187, #2587 ) ;
#16264 = CARTESIAN_POINT ( 'NONE',  ( 16.54345861550681107, 19.37554510112122230, -218.2240151908141002 ) ) ;
#16265 = CARTESIAN_POINT ( 'NONE',  ( 17.83206265427627457, -15.38023228143295640, -231.0294926223175480 ) ) ;
#16266 = CARTESIAN_POINT ( 'NONE',  ( 0.000000000000000000, -17.50000000000001066, -55.00000000000000711 ) ) ;
#16267 = CARTESIAN_POINT ( 'NONE',  ( -5.178973235464019886, -24.35492185057628944, -233.6431870320687381 ) ) ;
#16268 = SHAPE_DEFINITION_REPRESENTATION ( #3480, #1546 ) ;
#16269 = CARTESIAN_POINT ( 'NONE',  ( -3.082945806077231676, 30.69897765966285874, -224.2387254578930822 ) ) ;
#16270 = CARTESIAN_POINT ( 'NONE',  ( -0.2758005215353623862, 11.79991891162212525, -226.8645588387054488 ) ) ;
#16271 = ORIENTED_EDGE ( 'NONE', *, *, #8163, .T. ) ;
#16272 = CARTESIAN_POINT ( 'NONE',  ( -9.171998067665157350, 9.395241133357435714, -226.3428046914542051 ) ) ;
#16273 = CARTESIAN_POINT ( 'NONE',  ( -15.33992272861872763, -7.600289318192222865, -231.6130094852651951 ) ) ;
#16274 = CARTESIAN_POINT ( 'NONE',  ( -24.65527973750573665, -4.148457894541834001, 9.104741959888016822 ) ) ;
#16275 = CARTESIAN_POINT ( 'NONE',  ( -22.96373804598209389, 1.332909331808050490, -9.916358630100157612 ) ) ;
#16276 = CARTESIAN_POINT ( 'NONE',  ( -10.65455960636934662, 10.37188583052882862, -219.5197110153079620 ) ) ;
#16277 = CARTESIAN_POINT ( 'NONE',  ( -18.48589171870721870, -21.38265182533571362, -233.2911668074952729 ) ) ;
#16278 = AXIS2_PLACEMENT_3D ( 'NONE', #16177, #14280, #17978 ) ;
#16279 = CARTESIAN_POINT ( 'NONE',  ( 16.50235023187294203, -3.000022380394500310, -230.0447763498268614 ) ) ;
#16280 = CARTESIAN_POINT ( 'NONE',  ( -17.65835845419170624, 22.55329142274348442, -231.2673511165784532 ) ) ;
#16281 = CIRCLE ( 'NONE', #15573, 3.000000000000002665 ) ;
#16282 = CARTESIAN_POINT ( 'NONE',  ( -12.10179538005628963, 1.685214252672075030, -222.4835512146784424 ) ) ;
#16283 = CARTESIAN_POINT ( 'NONE',  ( -1.973645837583506424, 28.78841935349527503, -228.5341874691134763 ) ) ;
#16284 = CARTESIAN_POINT ( 'NONE',  ( 13.58841164691136427, 0.2900218890822029993, -227.9866932315656243 ) ) ;
#16285 = CARTESIAN_POINT ( 'NONE',  ( 15.80790828609669951, 3.698719088746416972, -219.8106174092292804 ) ) ;
#16286 = CARTESIAN_POINT ( 'NONE',  ( -8.398697845537501649, -22.62202615048447640, -219.0766901614751703 ) ) ;
#16287 = VERTEX_POINT ( 'NONE', #883 ) ;
#16288 = CARTESIAN_POINT ( 'NONE',  ( 10.31623634631035991, 26.83927646318382898, -220.2315638557092541 ) ) ;
#16289 = CARTESIAN_POINT ( 'NONE',  ( -5.854583994961135573, 13.10358817970001866, -222.4168379437668648 ) ) ;
#16290 = CARTESIAN_POINT ( 'NONE',  ( -21.29946384424354733, 21.01772963953914442, -222.5871995662667757 ) ) ;
#16291 = CARTESIAN_POINT ( 'NONE',  ( -26.61609457609114315, -10.18835510800150779, -222.8381276585760702 ) ) ;
#16292 = CARTESIAN_POINT ( 'NONE',  ( 0.000000000000000000, -17.50000000000000711, -55.00000000000000000 ) ) ;
#16293 = ORIENTED_EDGE ( 'NONE', *, *, #15077, .T. ) ;
#16294 = CARTESIAN_POINT ( 'NONE',  ( -28.99926036811508467, 3.909990568804979194, -228.9613767892386988 ) ) ;
#16295 = CARTESIAN_POINT ( 'NONE',  ( -5.902345112435694041, -11.50736153130091388, -224.0878888885884805 ) ) ;
#16296 = CARTESIAN_POINT ( 'NONE',  ( 13.45886389386542525, 0.9032831457644521223, -227.8643385330375963 ) ) ;
#16297 = CARTESIAN_POINT ( 'NONE',  ( -9.716674560061926869, 27.56227806819028103, -219.4917914922789919 ) ) ;
#16298 = PLANE ( 'NONE',  #14157 ) ;
#16299 = AXIS2_PLACEMENT_3D ( 'NONE', #7639, #7752, #17992 ) ;
#16300 = AXIS2_PLACEMENT_3D ( 'NONE', #5588, #635, #7404 ) ;
#16301 = CARTESIAN_POINT ( 'NONE',  ( 20.09685469220202236, -2.033783885649083079, -233.1448060988079760 ) ) ;
#16302 = CARTESIAN_POINT ( 'NONE',  ( 10.61539692146153691, 8.157890242340682718, -227.5705019877536301 ) ) ;
#16303 = EDGE_CURVE ( 'NONE', #3682, #8407, #5931, .T. ) ;
#16304 = CARTESIAN_POINT ( 'NONE',  ( 16.38151749656409351, 8.902090001712490874, -231.2955017965201989 ) ) ;
#16305 = CARTESIAN_POINT ( 'NONE',  ( -4.100000000000000533, 5.021051876504148371E-16, -75.00000000000000000 ) ) ;
#16306 = CARTESIAN_POINT ( 'NONE',  ( -13.09367826499460818, -1.871088059101057244, -230.2970504731880510 ) ) ;
#16307 = CARTESIAN_POINT ( 'NONE',  ( -15.46269062504165781, -26.67469327287815517, -225.2085449711190677 ) ) ;
#16308 = DIRECTION ( 'NONE',  ( 1.000000000000000000, 0.000000000000000000, 0.000000000000000000 ) ) ;
#16309 = FACE_OUTER_BOUND ( 'NONE', #5283, .T. ) ;
#16310 = CARTESIAN_POINT ( 'NONE',  ( -14.12265793148702464, 24.49085167151569919, -218.3312790639385241 ) ) ;
#16311 = CARTESIAN_POINT ( 'NONE',  ( 22.53017539111736411, -13.33152463597901516, -234.4848520764015518 ) ) ;
#16312 = CIRCLE ( 'NONE', #2993, 3.000000000000002665 ) ;
#16313 = CARTESIAN_POINT ( 'NONE',  ( 17.95694455891925756, -3.510678534943489026, -231.2643001502910067 ) ) ;
#16314 = CARTESIAN_POINT ( 'NONE',  ( -14.06164063153489252, 2.050767714179807744, -227.2881998904968270 ) ) ;
#16315 = CARTESIAN_POINT ( 'NONE',  ( 12.96449997971774870, 8.285709878278680662, -230.9518598506670628 ) ) ;
#16316 = CARTESIAN_POINT ( 'NONE',  ( 11.27486163995310164, 25.12851252939060487, -222.6718455410222930 ) ) ;
#16317 = ORIENTED_EDGE ( 'NONE', *, *, #12948, .T. ) ;
#16318 = CARTESIAN_POINT ( 'NONE',  ( 2.219167932009094901, -23.00164214691015729, -217.1940376169840476 ) ) ;
#16319 = CARTESIAN_POINT ( 'NONE',  ( 0.1235481402557489783, 14.50024104873819830, 92.99999999999998579 ) ) ;
#16320 = CARTESIAN_POINT ( 'NONE',  ( -6.111257124579617894, 15.89946952501658295, -216.3497764690875727 ) ) ;
#16321 = CARTESIAN_POINT ( 'NONE',  ( -4.378220565073127624, 31.53459173284372952, -222.0564199190954753 ) ) ;
#16322 = CARTESIAN_POINT ( 'NONE',  ( 26.90273745076186884, -10.52087603942467808, -226.9519702360728957 ) ) ;
#16323 = CARTESIAN_POINT ( 'NONE',  ( -3.205260335674071648, 17.52234722004434531, -232.9754319808710363 ) ) ;
#16324 = DIRECTION ( 'NONE',  ( 0.000000000000000000, 0.000000000000000000, 1.000000000000000000 ) ) ;
#16325 = CARTESIAN_POINT ( 'NONE',  ( -2.917590128672695293, 18.81591489065672818, -216.3635620530855022 ) ) ;
#16326 = CARTESIAN_POINT ( 'NONE',  ( 22.69522586737246783, 3.669837464059151344, -234.0947686933411944 ) ) ;
#16327 = CARTESIAN_POINT ( 'NONE',  ( -17.79285498209129202, 9.187865686019035749, -216.3798185811636756 ) ) ;
#16328 = VECTOR ( 'NONE', #10331, 1000.000000000000000 ) ;
#16329 = CARTESIAN_POINT ( 'NONE',  ( 14.19800769603076240, 4.587407146151301518, -224.2928935459285071 ) ) ;
#16330 = DIRECTION ( 'NONE',  ( -1.000000000000000000, -6.982962677686266711E-15, -0.000000000000000000 ) ) ;
#16331 = VERTEX_POINT ( 'NONE', #21241 ) ;
#16332 = CARTESIAN_POINT ( 'NONE',  ( -1.973645837583506424, 28.78841935349527503, -228.5341874691134763 ) ) ;
#16333 = CARTESIAN_POINT ( 'NONE',  ( -13.22951852716680676, -5.246159916193459338, -223.7538483380451453 ) ) ;
#16334 = CARTESIAN_POINT ( 'NONE',  ( 21.39553407250273054, 8.453402029343234148, -217.9531594780983141 ) ) ;
#16335 = CARTESIAN_POINT ( 'NONE',  ( 0.5573677079071300833, -14.80782849724859496, -218.9269569601107719 ) ) ;
#16336 = LINE ( 'NONE', #9259, #9588 ) ;
#16337 = CARTESIAN_POINT ( 'NONE',  ( -18.74633356284308761, 11.17209001323738704, -217.5809474206552068 ) ) ;
#16338 =( NAMED_UNIT ( * ) PLANE_ANGLE_UNIT ( ) SI_UNIT ( $, .RADIAN. ) );
#16339 = CARTESIAN_POINT ( 'NONE',  ( 9.020349274477036161, -13.22217574948208529, -220.4173403795374213 ) ) ;
#16340 = CARTESIAN_POINT ( 'NONE',  ( 15.28499842775873319, 22.98894588155567931, -221.0942409093412095 ) ) ;
#16341 = CARTESIAN_POINT ( 'NONE',  ( -21.23733589435050817, 17.25275849955597351, -229.9547908233139708 ) ) ;
#16342 = CARTESIAN_POINT ( 'NONE',  ( -13.91932826323387395, 8.983986115891950064, -216.4624824187541776 ) ) ;
#16343 = CARTESIAN_POINT ( 'NONE',  ( -16.98436007432217920, -11.01716238098750544, -231.0196200964405193 ) ) ;
#16344 =( REPRESENTATION_RELATIONSHIP ('NONE','NONE', #5277, #6134 ) REPRESENTATION_RELATIONSHIP_WITH_TRANSFORMATION ( #18398 )SHAPE_REPRESENTATION_RELATIONSHIP( ) );
#16345 = CARTESIAN_POINT ( 'NONE',  ( 24.00840102751045890, 17.37402299239434100, -218.3110108534040137 ) ) ;
#16346 = PRODUCT_DEFINITION ( 'UNKNOWN', '', #13534, #11672 ) ;
#16347 =( GEOMETRIC_REPRESENTATION_CONTEXT ( 3 ) GLOBAL_UNCERTAINTY_ASSIGNED_CONTEXT ( ( #21128 ) ) GLOBAL_UNIT_ASSIGNED_CONTEXT ( ( #8197, #18217, #6272 ) ) REPRESENTATION_CONTEXT ( 'NONE', 'WORKASPACE' ) );
#16348 = DIRECTION ( 'NONE',  ( -0.000000000000000000, -0.000000000000000000, -1.000000000000000000 ) ) ;
#16349 = CARTESIAN_POINT ( 'NONE',  ( -12.17842630902860712, -4.030040138803427929, -228.6515579410213661 ) ) ;
#16350 = CARTESIAN_POINT ( 'NONE',  ( 10.03842945413050458, 28.43460431997513638, -225.8374938385031214 ) ) ;
#16351 = CARTESIAN_POINT ( 'NONE',  ( 28.03290210476798094, 13.48017620089690638, -224.9212082181537937 ) ) ;
#16352 = CARTESIAN_POINT ( 'NONE',  ( -6.388048297418547961, 21.92257289597608150, -233.3290245341164848 ) ) ;
#16353 = CARTESIAN_POINT ( 'NONE',  ( 10.46530733675539793, 8.351728317179080818, -222.7431177495969621 ) ) ;
#16354 = CARTESIAN_POINT ( 'NONE',  ( 3.242550426224029447, -16.70085388461110654, -229.1030317736733650 ) ) ;
#16355 = CARTESIAN_POINT ( 'NONE',  ( -0.3025942668150596315, -28.96010673020088788, -223.5534481764385646 ) ) ;
#16356 = CARTESIAN_POINT ( 'NONE',  ( 17.00168025137501004, 6.212099629982537508, -219.0548246536471595 ) ) ;
#16357 = CARTESIAN_POINT ( 'NONE',  ( 19.68037530048075112, -17.97179847169212508, -231.8517058357153076 ) ) ;
#16358 = CARTESIAN_POINT ( 'NONE',  ( -15.15819830826754355, -2.370657588173597841, -221.8013720140894236 ) ) ;
#16359 = CIRCLE ( 'NONE', #6661, 21.63401512838748175 ) ;
#16360 = CARTESIAN_POINT ( 'NONE',  ( -5.240862053303020573, -11.96147391800445270, -224.1453450823045443 ) ) ;
#16361 = AXIS2_PLACEMENT_3D ( 'NONE', #506, #16145, #7382 ) ;
#16362 = CARTESIAN_POINT ( 'NONE',  ( 3.673290835002071653, 15.92545533070904895, -226.4848186297188022 ) ) ;
#16363 = FILL_AREA_STYLE_COLOUR ( '', #13139 ) ;
#16364 = CARTESIAN_POINT ( 'NONE',  ( -26.41026844077819291, 5.012316129610852933, -233.8406020309487872 ) ) ;
#16365 = CARTESIAN_POINT ( 'NONE',  ( 0.7245137624042983227, 13.44764381486384330, -223.4043886706536455 ) ) ;
#16366 = CARTESIAN_POINT ( 'NONE',  ( 7.042184411928968935, 23.28260216771182556, -230.5707103145148267 ) ) ;
#16367 = CARTESIAN_POINT ( 'NONE',  ( 29.52516483900593158, -0.1522717672070824924, -221.3034020690409704 ) ) ;
#16368 = ORIENTED_EDGE ( 'NONE', *, *, #485, .F. ) ;
#16369 = CARTESIAN_POINT ( 'NONE',  ( 25.62718606866737403, 13.33219119508369310, -230.9315691959737933 ) ) ;
#16370 = CARTESIAN_POINT ( 'NONE',  ( -25.36936018126600345, 11.57160208538938306, -224.9662154788713622 ) ) ;
#16371 = CARTESIAN_POINT ( 'NONE',  ( -22.18165477997343871, 9.502253276305026475, -218.0070055737419636 ) ) ;
#16372 = CARTESIAN_POINT ( 'NONE',  ( -1.615718423935818437, -15.01490656935555812, -223.2481059054151729 ) ) ;
#16373 = DIRECTION ( 'NONE',  ( 0.000000000000000000, 0.000000000000000000, 1.000000000000000000 ) ) ;
#16374 = CARTESIAN_POINT ( 'NONE',  ( 13.03557269046774714, 7.519834803053426775, -226.9490612297269081 ) ) ;
#16375 = CARTESIAN_POINT ( 'NONE',  ( 11.76368234164141136, -12.26645877504561888, -220.6132173800162946 ) ) ;
#16376 = DIRECTION ( 'NONE',  ( 0.000000000000000000, 0.000000000000000000, 1.000000000000000000 ) ) ;
#16377 = AXIS2_PLACEMENT_3D ( 'NONE', #15794, #7129, #21057 ) ;
#16378 = CARTESIAN_POINT ( 'NONE',  ( -1.489322793389167288, -21.37773154815333498, -215.8826219457350817 ) ) ;
#16379 = DIRECTION ( 'NONE',  ( 1.000000000000000000, 0.000000000000000000, 0.000000000000000000 ) ) ;
#16380 = CARTESIAN_POINT ( 'NONE',  ( -6.474151797443945533, 21.29193859232740138, -215.9573456447696458 ) ) ;
#16381 = CARTESIAN_POINT ( 'NONE',  ( 0.6332696906856497554, 18.74964962670039625, -234.8596399859513042 ) ) ;
#16382 = EDGE_LOOP ( 'NONE', ( #5216, #21843, #12504, #13638 ) ) ;
#16383 = CARTESIAN_POINT ( 'NONE',  ( -7.429838964355703901, 14.87322129099639234, -232.2632863647814077 ) ) ;
#16384 = CARTESIAN_POINT ( 'NONE',  ( -13.83093441725390704, -7.146379636134302160, -230.0501880019394605 ) ) ;
#16385 = CARTESIAN_POINT ( 'NONE',  ( -24.11485229701111166, -6.610722576001652584, 7.531077992868392634 ) ) ;
#16386 = DIRECTION ( 'NONE',  ( 0.000000000000000000, 0.000000000000000000, -1.000000000000000000 ) ) ;
#16387 = CARTESIAN_POINT ( 'NONE',  ( -9.716674560061926869, 27.56227806819028103, -219.4917914922789919 ) ) ;
#16388 = CARTESIAN_POINT ( 'NONE',  ( -3.350277215847999202, -25.10023987965119119, -233.9767109426786647 ) ) ;
#16390 = ADVANCED_FACE ( 'NONE', ( #7761 ), #18514, .T. ) ;
#16389 = CARTESIAN_POINT ( 'NONE',  ( 0.000000000000000000, 0.000000000000000000, 69.99999999999998579 ) ) ;
#16391 = CARTESIAN_POINT ( 'NONE',  ( -9.250876228778270871, 9.538614635316015722, -227.1332118982684563 ) ) ;
#16392 = CARTESIAN_POINT ( 'NONE',  ( -17.17143024911216287, 2.756036084795755681, -233.9491886983466316 ) ) ;
#16393 = CARTESIAN_POINT ( 'NONE',  ( 5.646952844456516019, 23.06006924884521325, -218.8221376988549878 ) ) ;
#16394 = CARTESIAN_POINT ( 'NONE',  ( 0.000000000000000000, 0.000000000000000000, -55.00000000000000000 ) ) ;
#16395 = CARTESIAN_POINT ( 'NONE',  ( 27.66944030902029539, 6.857614156517904291, -220.9860880211026313 ) ) ;
#16396 = CARTESIAN_POINT ( 'NONE',  ( -8.507271545618831254, -16.45592803179997787, -230.0780227380557790 ) ) ;
#16397 = TOROIDAL_SURFACE ( 'NONE', #19261, 22.63401512838748175, 3.000000000000002665 ) ;
#16398 = ORIENTED_EDGE ( 'NONE', *, *, #10094, .F. ) ;
#16399 =( GEOMETRIC_REPRESENTATION_CONTEXT ( 3 ) GLOBAL_UNCERTAINTY_ASSIGNED_CONTEXT ( ( #9224 ) ) GLOBAL_UNIT_ASSIGNED_CONTEXT ( ( #16556, #16338, #2597 ) ) REPRESENTATION_CONTEXT ( 'NONE', 'WORKASPACE' ) );
#16400 = CARTESIAN_POINT ( 'NONE',  ( 8.554868430186942874, 10.42313681336814568, -223.0114508542762621 ) ) ;
#16401 = CARTESIAN_POINT ( 'NONE',  ( 3.001892273201697048, 27.20292285420111966, -216.7800154582108689 ) ) ;
#16402 = VERTEX_POINT ( 'NONE', #11025 ) ;
#16403 = CARTESIAN_POINT ( 'NONE',  ( -29.01652113304903935, -3.607535226192160049, -222.1063433863846228 ) ) ;
#16404 = DIRECTION ( 'NONE',  ( 0.000000000000000000, -1.000000000000000000, 0.000000000000000000 ) ) ;
#16405 = EDGE_LOOP ( 'NONE', ( #11551, #17730, #20964, #4860 ) ) ;
#16406 = CARTESIAN_POINT ( 'NONE',  ( 16.56146809408446430, -0.9616313295950813522, -228.5729530379900609 ) ) ;
#16407 = CARTESIAN_POINT ( 'NONE',  ( 10.02513374692848913, 18.81568788741115128, -217.1505009242214612 ) ) ;
#16408 = CARTESIAN_POINT ( 'NONE',  ( -3.174954051807135080, -13.80109495427747746, -226.5796556275459750 ) ) ;
#16409 = CARTESIAN_POINT ( 'NONE',  ( 27.75679124201660741, 4.911524026080384075, -221.4430403652340829 ) ) ;
#16410 = CARTESIAN_POINT ( 'NONE',  ( 1.217121169770782663, 15.31158828575123110, -230.6845728599757308 ) ) ;
#16411 = DIRECTION ( 'NONE',  ( 0.000000000000000000, 0.000000000000000000, 1.000000000000000000 ) ) ;
#16412 = UNCERTAINTY_MEASURE_WITH_UNIT (LENGTH_MEASURE( 1.000000000000000082E-05 ), #9478, 'distance_accuracy_value', 'NONE');
#16413 = CIRCLE ( 'NONE', #3822, 14.50000000000000000 ) ;
#16414 = CARTESIAN_POINT ( 'NONE',  ( -26.47320305716024791, 9.675235842009668019, -228.3542180911597654 ) ) ;
#16415 = CARTESIAN_POINT ( 'NONE',  ( 19.66122710937851537, 22.83208755991274330, -220.0578523118790883 ) ) ;
#16416 = DIRECTION ( 'NONE',  ( 0.000000000000000000, 0.000000000000000000, -1.000000000000000000 ) ) ;
#16417 = CARTESIAN_POINT ( 'NONE',  ( 12.85408565574548412, 7.821283853063205171, -223.1248833997948111 ) ) ;
#16418 = FACE_OUTER_BOUND ( 'NONE', #17266, .T. ) ;
#16419 = CARTESIAN_POINT ( 'NONE',  ( 25.63739587761438088, -9.098054415140415685, -222.2988516439644968 ) ) ;
#16421 = EDGE_CURVE ( 'NONE', #16736, #9212, #18884, .T. ) ;
#16420 = CARTESIAN_POINT ( 'NONE',  ( -13.21314811618155716, -9.038438575223175064, -230.6430079410957603 ) ) ;
#16422 = CARTESIAN_POINT ( 'NONE',  ( -22.88757527474730580, -2.294270667724057855, -9.738816109291027701 ) ) ;
#16423 = CARTESIAN_POINT ( 'NONE',  ( -23.00000000000008882, 0.000000000000000000, 75.00000000000000000 ) ) ;
#16424 = CARTESIAN_POINT ( 'NONE',  ( -1.707778556226592581, 19.51307486516442680, -232.5708079709245055 ) ) ;
#16425 = CARTESIAN_POINT ( 'NONE',  ( 26.81360599170068326, -17.93330511230891844, -224.0089312182945491 ) ) ;
#16426 = CARTESIAN_POINT ( 'NONE',  ( 18.22947608839760747, -6.525328669204546905, -217.7409786913911205 ) ) ;
#16427 = CARTESIAN_POINT ( 'NONE',  ( -26.11114532382342901, 12.73400870066318902, -227.7653936945517046 ) ) ;
#16428 = CARTESIAN_POINT ( 'NONE',  ( 8.554868430186942874, 10.42313681336814568, -223.0114508542762621 ) ) ;
#16429 = CARTESIAN_POINT ( 'NONE',  ( 13.96918721733258195, 14.12724320058294403, -230.4946432816737172 ) ) ;
#16430 = VERTEX_POINT ( 'NONE', #13038 ) ;
#16431 = CARTESIAN_POINT ( 'NONE',  ( 6.264370104348762069, -18.85623240742893714, -216.4903287596617076 ) ) ;
#16432 = CARTESIAN_POINT ( 'NONE',  ( 0.000000000000000000, 0.000000000000000000, 77.51594804401857175 ) ) ;
#16433 = CARTESIAN_POINT ( 'NONE',  ( -5.543543819386913540, 14.51457927969963713, -217.3847528063896846 ) ) ;
#16434 = CARTESIAN_POINT ( 'NONE',  ( -19.90771709537278156, 23.83218599423810602, -225.0439263757368735 ) ) ;
#16435 = CARTESIAN_POINT ( 'NONE',  ( 19.99722954683925025, -4.901308424099491745, -217.6076555004800070 ) ) ;
#16436 = EDGE_CURVE ( 'NONE', #20364, #1644, #16359, .T. ) ;
#16437 = CARTESIAN_POINT ( 'NONE',  ( -2.698926868850080041, 12.89339462271858316, -226.7595176699009585 ) ) ;
#16438 = DIRECTION ( 'NONE',  ( -0.000000000000000000, -0.000000000000000000, -1.000000000000000000 ) ) ;
#16439 = EDGE_CURVE ( 'NONE', #6126, #15108, #3407, .T. ) ;
#16440 = CARTESIAN_POINT ( 'NONE',  ( 0.8673818989965740300, 28.69424263383094598, -231.7310846804014659 ) ) ;
#16441 = CARTESIAN_POINT ( 'NONE',  ( 13.49694890958685711, 2.186465430673721677, -228.8273158381700512 ) ) ;
#16442 = CARTESIAN_POINT ( 'NONE',  ( -11.46843428684449151, 6.508406145394057596, -225.7212143570321814 ) ) ;
#16443 = CARTESIAN_POINT ( 'NONE',  ( 22.86997486125673618, 17.56009411325475966, -222.3578648042903296 ) ) ;
#16444 = CARTESIAN_POINT ( 'NONE',  ( 8.321021197036545303, 25.59447019508656140, -228.6184429848799482 ) ) ;
#16445 = CARTESIAN_POINT ( 'NONE',  ( 15.62880906446489959, 0.6839391200676235849, -227.9224688803754475 ) ) ;
#16446 = EDGE_LOOP ( 'NONE', ( #3633, #5077, #2000, #15334 ) ) ;
#16447 = CARTESIAN_POINT ( 'NONE',  ( 5.549682179574114471, 15.11687613544382280, -226.9959476502473308 ) ) ;
#16448 = CARTESIAN_POINT ( 'NONE',  ( -19.50907964299920039, -17.77536300509877876, -217.8007844881196320 ) ) ;
#16449 = CARTESIAN_POINT ( 'NONE',  ( 16.84848658399567611, 11.39632653812981644, -217.9589513831453473 ) ) ;
#16450 = CARTESIAN_POINT ( 'NONE',  ( -3.624336683137088677, -15.65024371637965039, -218.6393395577867977 ) ) ;
#16451 = LINE ( 'NONE', #11053, #10292 ) ;
#16452 = CARTESIAN_POINT ( 'NONE',  ( -20.47640197314466093, 18.50423766437512541, -220.4440130802851456 ) ) ;
#16453 = CARTESIAN_POINT ( 'NONE',  ( 0.000000000000000000, 0.000000000000000000, -55.00000000000000000 ) ) ;
#16454 = CARTESIAN_POINT ( 'NONE',  ( 24.96165930385824794, -17.14663603160204275, -224.2745859498249672 ) ) ;
#16455 = CARTESIAN_POINT ( 'NONE',  ( 6.173705828530630768, 14.85108299334794957, -222.6284669816953112 ) ) ;
#16456 = CARTESIAN_POINT ( 'NONE',  ( -19.65084584916038324, 18.01805631773661176, -219.5040736310571106 ) ) ;
#16457 = CARTESIAN_POINT ( 'NONE',  ( -26.09112266552012471, 5.807188091516064077, -215.7774933166620883 ) ) ;
#16458 = CARTESIAN_POINT ( 'NONE',  ( -24.91054099106560926, -7.366054470814448862, -220.6971974931307159 ) ) ;
#16459 = CARTESIAN_POINT ( 'NONE',  ( 19.48863273024974418, 12.80680990455712909, -215.0408095016468053 ) ) ;
#16460 = PLANE ( 'NONE',  #18801 ) ;
#16461 = CARTESIAN_POINT ( 'NONE',  ( -15.25474278246548643, -4.999135024540048988, -232.7276810733381183 ) ) ;
#16462 = CARTESIAN_POINT ( 'NONE',  ( 2.630208337444488453, 16.40323635460054774, -219.2570070657488088 ) ) ;
#16463 = CARTESIAN_POINT ( 'NONE',  ( 21.04928763009552384, -0.2309942901367783852, -233.9427286327411366 ) ) ;
#16464 = CARTESIAN_POINT ( 'NONE',  ( -5.529079411693809121, 13.00503897727793401, -226.8014833675713646 ) ) ;
#16465 = CARTESIAN_POINT ( 'NONE',  ( 10.39636392256998221, 18.46527700675686035, -215.1860221565626148 ) ) ;
#16466 = CARTESIAN_POINT ( 'NONE',  ( 4.144298419883110540, -16.00443160190133085, -221.4341300285535965 ) ) ;
#16467 = CARTESIAN_POINT ( 'NONE',  ( 4.788325992165110456, -24.70830725884669121, -218.5516572218182603 ) ) ;
#16468 = CARTESIAN_POINT ( 'NONE',  ( 17.07668571305246985, 2.037405138410691485, -219.7626854147787867 ) ) ;
#16469 = CARTESIAN_POINT ( 'NONE',  ( 15.50779141722566656, -5.694711448414747856, -219.6385356284298211 ) ) ;
#16470 = CARTESIAN_POINT ( 'NONE',  ( 22.24262848504226042, 2.205713500382400216, -232.7243927205662999 ) ) ;
#16471 = CARTESIAN_POINT ( 'NONE',  ( -11.36971918743327237, -8.287084598727400220, -223.1364763414170227 ) ) ;
#16472 = CARTESIAN_POINT ( 'NONE',  ( 7.804112641607792611, 19.76858558208418515, -218.6463059509973164 ) ) ;
#16473 = DIRECTION ( 'NONE',  ( 0.000000000000000000, 0.000000000000000000, -1.000000000000000000 ) ) ;
#16474 = CARTESIAN_POINT ( 'NONE',  ( 17.92683513449900445, 4.153309877386362814, -218.0960491240478234 ) ) ;
#16475 = CARTESIAN_POINT ( 'NONE',  ( 10.66614775643814994, 26.29080367171353672, -230.0818785118670178 ) ) ;
#16476 = CARTESIAN_POINT ( 'NONE',  ( -0.2748333203896175525, 17.57683079704640505, -221.1444293135629948 ) ) ;
#16477 = CARTESIAN_POINT ( 'NONE',  ( 12.91141610427636621, -26.43280511468161720, -217.7946055251781274 ) ) ;
#16478 = CARTESIAN_POINT ( 'NONE',  ( 12.95792863868717149, 16.83236386576623644, -216.3406066345214356 ) ) ;
#16479 = CARTESIAN_POINT ( 'NONE',  ( -11.13829636790841704, 14.30978168460582189, -218.6922574227322400 ) ) ;
#16480 = CARTESIAN_POINT ( 'NONE',  ( 20.92846067405557520, -2.114533307883533109, -233.2756072794335580 ) ) ;
#16481 = CARTESIAN_POINT ( 'NONE',  ( 2.179383121900682951, -16.00498718933496889, -221.0566978482307832 ) ) ;
#16482 = CARTESIAN_POINT ( 'NONE',  ( 0.000000000000000000, 0.000000000000000000, 77.51594804401857175 ) ) ;
#16483 = CARTESIAN_POINT ( 'NONE',  ( 0.000000000000000000, 0.000000000000000000, -30.00000000000000000 ) ) ;
#16484 = CARTESIAN_POINT ( 'NONE',  ( 14.54149994592679107, 8.070685273005897997, -229.7292930672863349 ) ) ;
#16485 = CARTESIAN_POINT ( 'NONE',  ( 14.67088464789753388, -9.947482835004686663, -220.6944058341955497 ) ) ;
#16486 = CARTESIAN_POINT ( 'NONE',  ( -14.58575946311604277, 2.190332613129932327, -228.6717927865686590 ) ) ;
#16487 = AXIS2_PLACEMENT_3D ( 'NONE', #3102, #16734, #20088 ) ;
#16488 = CARTESIAN_POINT ( 'NONE',  ( -9.294226473174397540, -12.00440878504259601, -219.6990993854437875 ) ) ;
#16489 = CARTESIAN_POINT ( 'NONE',  ( 5.343558017910363667, 26.29639771561252459, -218.1010331760174665 ) ) ;
#16490 = CARTESIAN_POINT ( 'NONE',  ( 4.952019330116582907, 28.88045068338265509, -217.6369327391592208 ) ) ;
#16491 = ORIENTED_EDGE ( 'NONE', *, *, #3842, .F. ) ;
#16492 = CARTESIAN_POINT ( 'NONE',  ( -9.517741096562200909, 20.63709896626785678, -234.1036702156204967 ) ) ;
#16493 = CARTESIAN_POINT ( 'NONE',  ( -14.33274213004767716, -3.240524307521291725, -229.5155949954044559 ) ) ;
#16494 = CARTESIAN_POINT ( 'NONE',  ( 30.05917755080113096, -2.930701380670650114, -221.3976229872638726 ) ) ;
#16495 = FACE_OUTER_BOUND ( 'NONE', #11957, .T. ) ;
#16496 = CARTESIAN_POINT ( 'NONE',  ( -8.501641725227710111, 25.47064987787527102, -217.3358698761548737 ) ) ;
#16497 = CARTESIAN_POINT ( 'NONE',  ( -7.264683844434491000, -10.24731347617596100, -229.2886802738593985 ) ) ;
#16498 = CARTESIAN_POINT ( 'NONE',  ( 16.08921376350389920, -2.840750994787607731, -229.5571464835293796 ) ) ;
#16499 = CARTESIAN_POINT ( 'NONE',  ( -12.78558550453068854, 7.693178343823584342, -230.0800953344970878 ) ) ;
#16500 = CARTESIAN_POINT ( 'NONE',  ( -11.30246491834384770, 5.534029070539333794, -225.8243940897388597 ) ) ;
#16501 = CARTESIAN_POINT ( 'NONE',  ( 5.079647427451626562, 16.77877517420371234, -220.7769382327915366 ) ) ;
#16502 = CARTESIAN_POINT ( 'NONE',  ( 16.26115440404298340, 3.800605480264513059, -219.2833057824682612 ) ) ;
#16503 = CARTESIAN_POINT ( 'NONE',  ( -7.461655027780660809, -14.63259296063595727, -227.5661480528262075 ) ) ;
#16504 = EDGE_LOOP ( 'NONE', ( #19538, #2642, #10487, #6372 ) ) ;
#16505 = EDGE_CURVE ( 'NONE', #3205, #20901, #3122, .T. ) ;
#16506 = CARTESIAN_POINT ( 'NONE',  ( -13.51406939156936104, 10.04301168678160749, -230.1761202643687056 ) ) ;
#16507 = CARTESIAN_POINT ( 'NONE',  ( 8.903385417657583289, 10.41040586594612272, -227.6527940987422198 ) ) ;
#16508 = CARTESIAN_POINT ( 'NONE',  ( -2.121548062149551495, 13.26065194155116345, -221.8830439064491884 ) ) ;
#16509 = CARTESIAN_POINT ( 'NONE',  ( 30.87761267810551757, -2.376991648450896388, -225.4116222034606949 ) ) ;
#16510 = CARTESIAN_POINT ( 'NONE',  ( 18.00000000000000000, 1.360023205165816762E-13, 0.000000000000000000 ) ) ;
#16511 = EDGE_LOOP ( 'NONE', ( #13987, #17335, #2809, #7038 ) ) ;
#16512 = CARTESIAN_POINT ( 'NONE',  ( -13.56774755469388616, 7.311522441667196226, -219.1912666243428021 ) ) ;
#16513 = CARTESIAN_POINT ( 'NONE',  ( -6.651864601267788224, -12.12497212411570580, -228.9083653044881714 ) ) ;
#16514 = CARTESIAN_POINT ( 'NONE',  ( 21.60524407607017849, 3.028118258437591415, -217.8361640396714449 ) ) ;
#16515 = CARTESIAN_POINT ( 'NONE',  ( 11.33210854356620523, 22.81476816607802149, -217.8536224460118262 ) ) ;
#16516 = CYLINDRICAL_SURFACE ( 'NONE', #13080, 3.000000000000002665 ) ;
#16517 = CARTESIAN_POINT ( 'NONE',  ( -24.53276002501160136, 17.12571705644413811, -226.2419685911331442 ) ) ;
#16518 = CARTESIAN_POINT ( 'NONE',  ( 12.58577552758108986, 11.40439409249366420, -217.4478085440898951 ) ) ;
#16519 = SURFACE_STYLE_USAGE ( .BOTH. , #13363 ) ;
#16520 = CYLINDRICAL_SURFACE ( 'NONE', #5506, 3.000000000000002665 ) ;
#16521 = CARTESIAN_POINT ( 'NONE',  ( 11.87982377808925527, 10.85265283465803421, -229.5027252913499183 ) ) ;
#16522 = CARTESIAN_POINT ( 'NONE',  ( 0.000000000000000000, 0.000000000000000000, -101.2940952255125922 ) ) ;
#16523 = CARTESIAN_POINT ( 'NONE',  ( 21.42236089941604860, -11.78161700756472641, -230.3636358161748490 ) ) ;
#16524 = CARTESIAN_POINT ( 'NONE',  ( -14.73155177304599306, -1.817590056890399763, -226.9769936995019748 ) ) ;
#16525 = CARTESIAN_POINT ( 'NONE',  ( -22.72510797543546346, -3.558559409777959370, -9.351142534105258974 ) ) ;
#16526 = DIRECTION ( 'NONE',  ( 0.000000000000000000, 0.000000000000000000, -1.000000000000000000 ) ) ;
#16527 = CARTESIAN_POINT ( 'NONE',  ( -1.470815287892122125, 29.54293232078718745, -224.5855911371830302 ) ) ;
#16528 = CARTESIAN_POINT ( 'NONE',  ( 12.30978816035033496, -6.276705103789536722, -231.2162571060900405 ) ) ;
#16529 = CARTESIAN_POINT ( 'NONE',  ( 24.05826999138443156, -14.97270453765939102, -220.1026142722873260 ) ) ;
#16530 = CARTESIAN_POINT ( 'NONE',  ( -27.52457542293397097, 5.447957517019466067, -230.2717933641555135 ) ) ;
#16531 = CARTESIAN_POINT ( 'NONE',  ( 29.55842656951424985, 4.785221541509360854, -220.5134865854112718 ) ) ;
#16532 = CARTESIAN_POINT ( 'NONE',  ( 15.20072702475037296, 19.31591084219522614, -219.7402199933931399 ) ) ;
#16533 = VERTEX_POINT ( 'NONE', #15406 ) ;
#16534 = CARTESIAN_POINT ( 'NONE',  ( -0.004649462380863607185, -15.32103018016390017, -221.8331694311728484 ) ) ;
#16535 = CARTESIAN_POINT ( 'NONE',  ( -10.07820250684337537, 10.42709000561872479, 92.99999999999998579 ) ) ;
#16536 = CARTESIAN_POINT ( 'NONE',  ( -13.63292518690856170, 3.968236334994402981, -218.3158317831635316 ) ) ;
#16537 = CARTESIAN_POINT ( 'NONE',  ( 13.09827881591457022, 28.40264942367575784, -221.1045935444571455 ) ) ;
#16538 = CARTESIAN_POINT ( 'NONE',  ( -0.6224962293416278492, 14.12372964796689701, -218.2103911528446645 ) ) ;
#16539 = CARTESIAN_POINT ( 'NONE',  ( 17.73959705210031146, -11.46016327460725748, -231.4839417819510459 ) ) ;
#16540 = CARTESIAN_POINT ( 'NONE',  ( 0.4042326456706432647, 15.50845657815858303, -219.2680337625893401 ) ) ;
#16541 = CARTESIAN_POINT ( 'NONE',  ( -15.15110768032078070, 3.517015312212880218, -219.5479300368539270 ) ) ;
#16542 = ADVANCED_FACE ( 'NONE', ( #8430 ), #13713, .F. ) ;
#16543 = CARTESIAN_POINT ( 'NONE',  ( -2.508488193221233953, 16.03207605874066033, -217.8880952293912969 ) ) ;
#16544 = CARTESIAN_POINT ( 'NONE',  ( -15.72195651633673208, 2.938252489821347346, -222.2698596109374023 ) ) ;
#16545 = CARTESIAN_POINT ( 'NONE',  ( -18.09776816382430908, 23.50806826204562583, -229.9568677523880638 ) ) ;
#16546 = CARTESIAN_POINT ( 'NONE',  ( 21.25094435758043332, 17.68230636442804027, -229.7964888993842010 ) ) ;
#16547 = CARTESIAN_POINT ( 'NONE',  ( 5.688640247940316641, 20.34961083808282822, -230.9155060479073711 ) ) ;
#16548 = FACE_OUTER_BOUND ( 'NONE', #21012, .T. ) ;
#16549 = EDGE_CURVE ( 'NONE', #14565, #9583, #19158, .T. ) ;
#16550 = CARTESIAN_POINT ( 'NONE',  ( 11.40028598017942230, 13.60807601628675023, -220.9105305289655519 ) ) ;
#16551 = CARTESIAN_POINT ( 'NONE',  ( -20.18470553695442860, -13.13924840112635195, -232.9662461559857718 ) ) ;
#16552 = CARTESIAN_POINT ( 'NONE',  ( 14.85123888640019452, 5.067529763532427012, -221.9058491819374979 ) ) ;
#16553 = CARTESIAN_POINT ( 'NONE',  ( -1.453954827973251929, -30.77017545459721859, -228.2950292831040713 ) ) ;
#16554 = DIRECTION ( 'NONE',  ( 0.000000000000000000, 1.000000000000000000, -0.000000000000000000 ) ) ;
#16555 = CARTESIAN_POINT ( 'NONE',  ( -4.879985665934096772, 15.33285679834440174, -220.9402849574511833 ) ) ;
#16556 =( LENGTH_UNIT ( ) NAMED_UNIT ( * ) SI_UNIT ( .MILLI., .METRE. ) );
#16557 = CARTESIAN_POINT ( 'NONE',  ( 19.19076252585518105, -11.68002947460017715, -233.4322573972352188 ) ) ;
#16558 = CARTESIAN_POINT ( 'NONE',  ( 20.85755584069816493, 20.53615333921957742, -227.2010381488614996 ) ) ;
#16559 = CARTESIAN_POINT ( 'NONE',  ( -11.16203726658389606, 26.27101666727781648, -227.8592829514190612 ) ) ;
#16560 = CARTESIAN_POINT ( 'NONE',  ( -13.55637112341987383, 4.614880311503475774, -231.8130385267184010 ) ) ;
#16561 = CARTESIAN_POINT ( 'NONE',  ( -13.13160344394316503, -9.470348871083606568, -223.0142826039989075 ) ) ;
#16562 = VECTOR ( 'NONE', #20872, 1000.000000000000000 ) ;
#16563 = CARTESIAN_POINT ( 'NONE',  ( -25.06333669508177309, 2.553070212212491530, -230.2963116797556893 ) ) ;
#16564 = DIRECTION ( 'NONE',  ( 1.000000000000000000, -3.552713678800500929E-15, 0.000000000000000000 ) ) ;
#16565 = CARTESIAN_POINT ( 'NONE',  ( -27.52442056016948868, -15.72718643249855397, -222.0944556419597689 ) ) ;
#16566 = CARTESIAN_POINT ( 'NONE',  ( 16.69977105456987232, 16.51652889326612694, -233.6667933521891030 ) ) ;
#16567 = CARTESIAN_POINT ( 'NONE',  ( 20.76808360334631232, 5.412616674732960931, -234.1222385626545304 ) ) ;
#16568 = CARTESIAN_POINT ( 'NONE',  ( 1.898427734299754421, 12.47096978853034521, -227.5043976727869506 ) ) ;
#16569 = CARTESIAN_POINT ( 'NONE',  ( 14.02309809840729393, 19.05079204846204277, -234.6885355850075143 ) ) ;
#16570 = EDGE_LOOP ( 'NONE', ( #19200, #510, #18536, #17951 ) ) ;
#16571 = CARTESIAN_POINT ( 'NONE',  ( 4.239709385547987708, -16.34504625405869405, -220.9645569933060756 ) ) ;
#16572 = VERTEX_POINT ( 'NONE', #16865 ) ;
#16573 = CARTESIAN_POINT ( 'NONE',  ( -5.429593058350183910, -25.95961553913046416, -230.5291520159703111 ) ) ;
#16574 = ADVANCED_FACE ( 'NONE', ( #1441 ), #4692, .F. ) ;
#16575 = CARTESIAN_POINT ( 'NONE',  ( -20.06846544527470400, 7.877362284741439069, -235.3910773253824402 ) ) ;
#16576 = CARTESIAN_POINT ( 'NONE',  ( 21.05631363308661363, -21.50266115212419393, -222.6654548186096747 ) ) ;
#16577 = CARTESIAN_POINT ( 'NONE',  ( -27.88251101234890328, -7.575382714962081820, -221.6715981084135478 ) ) ;
#16578 = CARTESIAN_POINT ( 'NONE',  ( -11.49803752765619258, -8.459563989871591971, -222.4296168992866853 ) ) ;
#16579 = CARTESIAN_POINT ( 'NONE',  ( 9.575488824002899690, 13.89846378187365694, -220.1158735840035945 ) ) ;
#16580 = CARTESIAN_POINT ( 'NONE',  ( 0.000000000000000000, 17.50000000000000711, -55.00000000000000000 ) ) ;
#16581 = CARTESIAN_POINT ( 'NONE',  ( -9.746008880186941781, 12.96562886885531896, -220.1990846131056401 ) ) ;
#16582 = CARTESIAN_POINT ( 'NONE',  ( 11.17884645811568944, 10.10284797925214662, -221.0856722371208036 ) ) ;
#16583 = CARTESIAN_POINT ( 'NONE',  ( 1.382955251742491898, 16.46353944795171032, -231.7743150979565030 ) ) ;
#16584 = CARTESIAN_POINT ( 'NONE',  ( 16.82251835652528982, 18.18719385133374544, -231.8032941011735772 ) ) ;
#16585 = CARTESIAN_POINT ( 'NONE',  ( 8.727084366397900084, -11.39314604550613375, -218.1375774943401495 ) ) ;
#16586 = CARTESIAN_POINT ( 'NONE',  ( 10.95881707662767290, 12.06788758096456782, -231.4359029166177208 ) ) ;
#16587 = CARTESIAN_POINT ( 'NONE',  ( -5.590964611773372894, 13.92546790642523113, -228.7941110425196882 ) ) ;
#16588 = CARTESIAN_POINT ( 'NONE',  ( 0.4703770282364683197, -28.19050476347214484, -228.5103440588500519 ) ) ;
#16589 = CARTESIAN_POINT ( 'NONE',  ( -29.95012366401462955, 4.746560250930182967, -224.6954343660969471 ) ) ;
#16590 = DIRECTION ( 'NONE',  ( 1.000000000000000000, 0.000000000000000000, 0.000000000000000000 ) ) ;
#16591 = AXIS2_PLACEMENT_3D ( 'NONE', #13559, #3180, #13978 ) ;
#16592 = CARTESIAN_POINT ( 'NONE',  ( 21.53262694368047647, 11.06794636811408594, -231.8394491640143826 ) ) ;
#16593 = CARTESIAN_POINT ( 'NONE',  ( 15.58552416334512536, -6.625011841737234342, -222.1645676924547104 ) ) ;
#16594 = DIRECTION ( 'NONE',  ( 0.000000000000000000, 0.000000000000000000, 1.000000000000000000 ) ) ;
#16595 = CARTESIAN_POINT ( 'NONE',  ( -6.642805165258356404, -28.12267032419628521, -230.9452027245340560 ) ) ;
#16596 = CARTESIAN_POINT ( 'NONE',  ( -3.514547081416551588, 30.38636916157537016, -227.3529586180979436 ) ) ;
#16597 = AXIS2_PLACEMENT_3D ( 'NONE', #12170, #14207, #7114 ) ;
#16598 = CARTESIAN_POINT ( 'NONE',  ( 5.501756899793208255, 15.97909684020861043, -233.9380718515096191 ) ) ;
#16599 = ORIENTED_EDGE ( 'NONE', *, *, #9431, .F. ) ;
#16600 = CARTESIAN_POINT ( 'NONE',  ( -2.208416658185406334, 29.10348627872611615, -219.8480645685746424 ) ) ;
#16601 = CARTESIAN_POINT ( 'NONE',  ( -28.74911369566071784, -10.37195270599671737, -225.4617258471509729 ) ) ;
#16602 = CARTESIAN_POINT ( 'NONE',  ( -24.11215523719795328, -6.608422274973745125, -7.512281027134874556 ) ) ;
#16603 = DIRECTION ( 'NONE',  ( -1.000000000000000000, 0.000000000000000000, 0.000000000000000000 ) ) ;
#16604 = CARTESIAN_POINT ( 'NONE',  ( 2.539761864897490007, 23.64215977235053501, -233.4645566207487661 ) ) ;
#16605 = CARTESIAN_POINT ( 'NONE',  ( -4.912481909026474192, -29.12074637257241250, -231.0965163926508410 ) ) ;
#16606 = CARTESIAN_POINT ( 'NONE',  ( 2.098184199980985376, -13.29281380427311099, -222.1652846463370281 ) ) ;
#16607 = CARTESIAN_POINT ( 'NONE',  ( 24.05826999138443156, -14.97270453765939102, -220.1026142722873260 ) ) ;
#16608 = AXIS2_PLACEMENT_3D ( 'NONE', #15668, #17467, #5181 ) ;
#16609 = CARTESIAN_POINT ( 'NONE',  ( 14.18323607655884722, 3.286047475533308226, -222.8710065128477140 ) ) ;
#16610 = CARTESIAN_POINT ( 'NONE',  ( 16.07044873961816123, 22.39643131523411412, -226.8512752114033901 ) ) ;
#16611 = CARTESIAN_POINT ( 'NONE',  ( -21.89482327431018760, 1.733733432562314158, -233.1353281693111796 ) ) ;
#16612 = CARTESIAN_POINT ( 'NONE',  ( -18.16160515720599022, 12.42447964075808997, -216.1086293678848449 ) ) ;
#16613 = CARTESIAN_POINT ( 'NONE',  ( -19.35484598183500538, -9.368503549647014594, -231.4111816933332477 ) ) ;
#16614 = EDGE_LOOP ( 'NONE', ( #4813, #9643, #13332, #1985, #671, #11735 ) ) ;
#16615 = CARTESIAN_POINT ( 'NONE',  ( -24.39036648059286350, 13.21953970265592027, -220.1632778389106591 ) ) ;
#16616 = CARTESIAN_POINT ( 'NONE',  ( 5.702651035983461902, 12.42242820409033222, -224.7304266323218656 ) ) ;
#16617 = CARTESIAN_POINT ( 'NONE',  ( 0.8673818989965740300, 28.69424263383094598, -231.7310846804014659 ) ) ;
#16618 = VECTOR ( 'NONE', #21921, 1000.000000000000000 ) ;
#16619 = CARTESIAN_POINT ( 'NONE',  ( -14.73475970555713310, -4.645830632990214148, -227.0446463473171832 ) ) ;
#16620 = CARTESIAN_POINT ( 'NONE',  ( -12.50000000000000355, 1.836970198721030378E-15, -70.00000000000000000 ) ) ;
#16621 = VERTEX_POINT ( 'NONE', #8313 ) ;
#16622 = CARTESIAN_POINT ( 'NONE',  ( -20.18153419852512442, 14.25141268122526483, -233.5059133483111964 ) ) ;
#16623 = CARTESIAN_POINT ( 'NONE',  ( -5.045022908720540045, -16.91549468467126616, -232.0765493255083243 ) ) ;
#16624 = CARTESIAN_POINT ( 'NONE',  ( 13.57284447417419493, 1.290488679629692381, -227.7116397237339811 ) ) ;
#16625 = CARTESIAN_POINT ( 'NONE',  ( 17.97843143658897347, 22.12221935793617078, -220.9346589834416079 ) ) ;
#16626 = FACE_BOUND ( 'NONE', #9629, .T. ) ;
#16627 = CARTESIAN_POINT ( 'NONE',  ( 14.02668320743028119, -5.282748560960272677, -221.9001732195871739 ) ) ;
#16628 = CARTESIAN_POINT ( 'NONE',  ( -15.23792247720107440, 7.806131751461257373, -230.3336101049160902 ) ) ;
#16629 = AXIS2_PLACEMENT_3D ( 'NONE', #5477, #21328, #5701 ) ;
#16630 = CARTESIAN_POINT ( 'NONE',  ( 27.16757474806794903, 2.676291341565463888, -220.8863403533574115 ) ) ;
#16631 = AXIS2_PLACEMENT_3D ( 'NONE', #7786, #11265, #14543 ) ;
#16632 = DIRECTION ( 'NONE',  ( -1.000000000000000000, 0.000000000000000000, 0.000000000000000000 ) ) ;
#16633 = EDGE_CURVE ( 'NONE', #9014, #7956, #14155, .T. ) ;
#16634 = CARTESIAN_POINT ( 'NONE',  ( 27.04607490430786854, 4.607450003618843049, -220.3758934308003461 ) ) ;
#16635 = DIRECTION ( 'NONE',  ( -1.000000000000000000, -1.224646799147353454E-16, 0.000000000000000000 ) ) ;
#16636 = CARTESIAN_POINT ( 'NONE',  ( 20.55466028792283240, -8.067975053177056211, -219.1472888552992799 ) ) ;
#16637 = CARTESIAN_POINT ( 'NONE',  ( -13.22951852716680676, -5.246159916193459338, -223.7538483380451453 ) ) ;
#16638 = CARTESIAN_POINT ( 'NONE',  ( 0.000000000000000000, 0.000000000000000000, -77.51594804401857175 ) ) ;
#16639 = DIRECTION ( 'NONE',  ( 0.000000000000000000, 1.000000000000000000, -0.000000000000000000 ) ) ;
#16640 = CARTESIAN_POINT ( 'NONE',  ( -4.813101935419741295, 13.68373293383429434, -229.7840611589179503 ) ) ;
#16641 = CARTESIAN_POINT ( 'NONE',  ( 27.82583766398256486, 0.7543585032809253521, -232.9329547162639358 ) ) ;
#16642 = CARTESIAN_POINT ( 'NONE',  ( 17.43540344723615476, -3.335533435063737340, -230.8961756483947738 ) ) ;
#16643 = CARTESIAN_POINT ( 'NONE',  ( -18.14952719657095415, 1.368063294522122275, -218.0005379682515922 ) ) ;
#16644 = CARTESIAN_POINT ( 'NONE',  ( 30.60340911705754863, 5.703403611927857497, -225.1938343315648297 ) ) ;
#16645 = CARTESIAN_POINT ( 'NONE',  ( 24.14003655968566520, 13.76285650325712773, -228.1266575292093819 ) ) ;
#16646 = CARTESIAN_POINT ( 'NONE',  ( 5.503098680704820111, -17.53359096179937993, -217.0817822229213618 ) ) ;
#16647 = CARTESIAN_POINT ( 'NONE',  ( 14.50000000000000000, 0.000000000000000000, 93.00000000000000000 ) ) ;
#16648 = AXIS2_PLACEMENT_3D ( 'NONE', #10043, #1480, #20710 ) ;
#16649 = CARTESIAN_POINT ( 'NONE',  ( -21.89065952084861522, -0.9940043559354512226, -215.0000000000000000 ) ) ;
#16650 = CIRCLE ( 'NONE', #6953, 1.000000000000000888 ) ;
#16651 = CARTESIAN_POINT ( 'NONE',  ( 17.04685026979186446, 18.05617612716381970, -216.0910122987878310 ) ) ;
#16652 = CARTESIAN_POINT ( 'NONE',  ( 9.100443535964535258, 24.01370002727352215, -234.5397711707082635 ) ) ;
#16653 = CARTESIAN_POINT ( 'NONE',  ( 14.78595257191855694, -4.705020206487795065, -221.9958499870062099 ) ) ;
#16654 = CARTESIAN_POINT ( 'NONE',  ( -5.807479211365208727, 19.77444019604324410, -216.0778658752277863 ) ) ;
#16655 = CARTESIAN_POINT ( 'NONE',  ( -25.61997837663875188, 10.01664178086244483, -231.6711741719404074 ) ) ;
#16656 = CARTESIAN_POINT ( 'NONE',  ( 12.75306435971521068, 14.56583715532477186, -214.9711136650476533 ) ) ;
#16657 = CARTESIAN_POINT ( 'NONE',  ( -17.89085717681497201, 10.08962028281416856, -232.3705156551908431 ) ) ;
#16658 = CARTESIAN_POINT ( 'NONE',  ( -3.368164009525018265, 19.03203264544105622, -233.5986411977714567 ) ) ;
#16659 = CARTESIAN_POINT ( 'NONE',  ( 21.35706335192880445, 15.67286272432725092, -219.2578158352350783 ) ) ;
#16660 = CIRCLE ( 'NONE', #3364, 2.000000000000000000 ) ;
#16661 = CARTESIAN_POINT ( 'NONE',  ( 10.64798096806036121, 19.48085866535796740, -231.3996658690317361 ) ) ;
#16662 = CIRCLE ( 'NONE', #21678, 3.000000000000002665 ) ;
#16663 = CARTESIAN_POINT ( 'NONE',  ( 14.56914850832129815, -2.041740472307377985, -224.7121590863160350 ) ) ;
#16664 = DIRECTION ( 'NONE',  ( -0.000000000000000000, -0.000000000000000000, 1.000000000000000000 ) ) ;
#16665 = CARTESIAN_POINT ( 'NONE',  ( -14.73155177304599306, -1.817590056890399763, -226.9769936995019748 ) ) ;
#16666 = CARTESIAN_POINT ( 'NONE',  ( 14.31308345469695453, 12.76656023072872159, -231.9445021321040770 ) ) ;
#16667 = CARTESIAN_POINT ( 'NONE',  ( -8.288471666609035893, -17.31860360376325403, -217.6655967056599366 ) ) ;
#16668 = DIRECTION ( 'NONE',  ( 4.845403715540889009E-30, -6.938893903907222461E-16, 1.000000000000000000 ) ) ;
#16669 = ADVANCED_FACE ( 'NONE', ( #8983 ), #13065, .T. ) ;
#16670 = CARTESIAN_POINT ( 'NONE',  ( -17.08384421609436643, 23.56421365837046622, -225.2902702884460666 ) ) ;
#16671 = CARTESIAN_POINT ( 'NONE',  ( 7.739744183733028748, -12.54214339878522999, -227.5419174737939159 ) ) ;
#16672 = CARTESIAN_POINT ( 'NONE',  ( 11.17884645811568944, 10.10284797925214662, -221.0856722371208036 ) ) ;
#16673 = CARTESIAN_POINT ( 'NONE',  ( -4.073886805163430935, 14.35067061637828623, -226.4733297826468572 ) ) ;
#16674 = CARTESIAN_POINT ( 'NONE',  ( -28.88770769694534479, 14.24820799418726480, -223.2044777450442155 ) ) ;
#16675 = CARTESIAN_POINT ( 'NONE',  ( -18.87172488519036762, -12.11125346135639802, -231.2159161446224402 ) ) ;
#16676 = CARTESIAN_POINT ( 'NONE',  ( -17.91769793922991028, 3.277678596821882007, -219.5526088240203819 ) ) ;
#16677 = CIRCLE ( 'NONE', #20616, 21.00000000000000000 ) ;
#16678 = PLANE ( 'NONE',  #9818 ) ;
#16679 = CARTESIAN_POINT ( 'NONE',  ( -30.16187987321119834, 0.7031948255570967810, -222.4584828387981474 ) ) ;
#16680 = CARTESIAN_POINT ( 'NONE',  ( 9.798337081649805214, 12.27506320122302697, -218.9346733583377613 ) ) ;
#16681 = AXIS2_PLACEMENT_3D ( 'NONE', #16720, #21989, #16603 ) ;
#16682 = CARTESIAN_POINT ( 'NONE',  ( -24.40185606299549192, 11.66496215664722236, -221.9473669705449765 ) ) ;
#16683 = CARTESIAN_POINT ( 'NONE',  ( -2.508488193221233953, 16.03207605874066033, -217.8880952293912969 ) ) ;
#16684 = CARTESIAN_POINT ( 'NONE',  ( 4.228809304811371739, 12.93497549386982470, -230.7917784105561907 ) ) ;
#16685 = CARTESIAN_POINT ( 'NONE',  ( -12.42003616114091358, -24.71691410793946986, -217.8239624370676779 ) ) ;
#16686 = VERTEX_POINT ( 'NONE', #422 ) ;
#16687 = CARTESIAN_POINT ( 'NONE',  ( 6.203932113039332563, -21.09630782756332223, -232.3325312104709894 ) ) ;
#16688 = CARTESIAN_POINT ( 'NONE',  ( -15.39319649241581800, 0.3563955590804028795, -232.4397289486159082 ) ) ;
#16689 = CARTESIAN_POINT ( 'NONE',  ( 24.05826999138443156, -14.97270453765939102, -220.1026142722873260 ) ) ;
#16690 = CARTESIAN_POINT ( 'NONE',  ( -21.80830016239255897, -4.781675611938959847, -217.4666014280278148 ) ) ;
#16691 = CARTESIAN_POINT ( 'NONE',  ( -5.804961988600464196, -12.67915086496026511, -228.7923277404792088 ) ) ;
#16692 = CARTESIAN_POINT ( 'NONE',  ( 23.08329078023534109, 11.96623404944238978, -217.1428499060670845 ) ) ;
#16693 = DIRECTION ( 'NONE',  ( 0.000000000000000000, 0.000000000000000000, 1.000000000000000000 ) ) ;
#16694 = CARTESIAN_POINT ( 'NONE',  ( -18.16160515720599022, 12.42447964075808997, -216.1086293678848449 ) ) ;
#16695 = CARTESIAN_POINT ( 'NONE',  ( 10.98110116949302828, 13.70618071521442971, -230.2797640191687378 ) ) ;
#16696 = TOROIDAL_SURFACE ( 'NONE', #3025, 22.63401512838748175, 3.000000000000002665 ) ;
#16697 = CARTESIAN_POINT ( 'NONE',  ( 9.333020543840051531, 16.91085096921651143, -217.7308990335875762 ) ) ;
#16698 = CARTESIAN_POINT ( 'NONE',  ( 11.17884645811568944, 10.10284797925214662, -221.0856722371208036 ) ) ;
#16699 = CARTESIAN_POINT ( 'NONE',  ( 7.844578353157877437, -11.10597526584381356, -230.9016046914076128 ) ) ;
#16700 = CARTESIAN_POINT ( 'NONE',  ( 14.33191776452776622, 5.147404080619256916, -219.0172570056664938 ) ) ;
#16701 = CARTESIAN_POINT ( 'NONE',  ( -11.11479000491124047, 20.76372272540567110, -218.2001872134434564 ) ) ;
#16702 = CARTESIAN_POINT ( 'NONE',  ( -7.266348978356541366, 16.38312187400933340, -217.9429203627011873 ) ) ;
#16703 = CARTESIAN_POINT ( 'NONE',  ( -17.01799258133205228, -17.74971190556693657, -217.5843211863294755 ) ) ;
#16704 = CARTESIAN_POINT ( 'NONE',  ( -28.59157645096996347, 5.137867505054540374, -220.4667042235044505 ) ) ;
#16705 = LINE ( 'NONE', #1285, #11926 ) ;
#16706 = CARTESIAN_POINT ( 'NONE',  ( 22.46220731426537043, 18.23201731183003460, -227.5436199598787539 ) ) ;
#16707 = CARTESIAN_POINT ( 'NONE',  ( 7.317916060359300978, -13.14109500694934951, -227.5371884182924305 ) ) ;
#16708 = CARTESIAN_POINT ( 'NONE',  ( -25.19248792833826300, 13.40115236862232528, -221.2817950683888455 ) ) ;
#16709 = EDGE_CURVE ( 'NONE', #15877, #6212, #7073, .T. ) ;
#16710 = CARTESIAN_POINT ( 'NONE',  ( -20.11874861854083463, -21.11755179634840474, -229.7504124090357323 ) ) ;
#16711 = EDGE_CURVE ( 'NONE', #12137, #137, #17642, .T. ) ;
#16712 = CARTESIAN_POINT ( 'NONE',  ( -20.86570240061152148, 1.122719768445835875, -219.0984131021933763 ) ) ;
#16713 = EDGE_CURVE ( 'NONE', #15809, #13837, #3898, .T. ) ;
#16715 = CARTESIAN_POINT ( 'NONE',  ( 4.228809304811371739, 12.93497549386982470, -230.7917784105561907 ) ) ;
#16714 = CIRCLE ( 'NONE', #1627, 19.79999999999999716 ) ;
#16716 = ORIENTED_EDGE ( 'NONE', *, *, #198, .T. ) ;
#16717 = CARTESIAN_POINT ( 'NONE',  ( -11.42613629117093765, 28.09170287990588832, -228.7150250545069241 ) ) ;
#16718 = CARTESIAN_POINT ( 'NONE',  ( 29.72361553920624999, -4.223772423702004453, -224.3921473884441866 ) ) ;
#16719 = CARTESIAN_POINT ( 'NONE',  ( -22.94848423520210901, -9.918082410655362224, 1.320023449481911415 ) ) ;
#16720 = CARTESIAN_POINT ( 'NONE',  ( 0.000000000000000000, 0.000000000000000000, 77.51594804401857175 ) ) ;
#16721 = CARTESIAN_POINT ( 'NONE',  ( 2.008896548638861024, 20.64812324442097591, -233.5818019448501843 ) ) ;
#16722 = CARTESIAN_POINT ( 'NONE',  ( -5.856318878364832337, -22.45395696943396402, -215.0711972856051943 ) ) ;
#16723 = CARTESIAN_POINT ( 'NONE',  ( 6.053458391837899910, -12.85229775019162268, -220.9645494416007523 ) ) ;
#16724 = CARTESIAN_POINT ( 'NONE',  ( 24.56541673123750158, -5.996287403333383281, -231.6940117905984664 ) ) ;
#16725 = CARTESIAN_POINT ( 'NONE',  ( -15.05930145804884290, 24.78193219970826533, -223.0510781988847953 ) ) ;
#16726 = CARTESIAN_POINT ( 'NONE',  ( 8.858651440950676914, 22.47383302477780376, -230.7859943773311215 ) ) ;
#16727 = DIRECTION ( 'NONE',  ( 0.000000000000000000, -1.000000000000000000, 0.000000000000000000 ) ) ;
#16728 = CARTESIAN_POINT ( 'NONE',  ( -20.04070223234628756, 18.12164545743767263, -231.9292141396248610 ) ) ;
#16729 = CARTESIAN_POINT ( 'NONE',  ( -15.55375487336196372, -9.676988738288478942, -219.9111427047364202 ) ) ;
#16730 = CARTESIAN_POINT ( 'NONE',  ( -11.08731210905863840, 25.61052584666692766, -228.9953606804266997 ) ) ;
#16731 = CARTESIAN_POINT ( 'NONE',  ( 18.81274554574540403, 10.85963742466947224, -234.0446454529665345 ) ) ;
#16732 = CARTESIAN_POINT ( 'NONE',  ( 7.283976506941576723, 24.82246917020504284, -234.3244871078919402 ) ) ;
#16733 = CARTESIAN_POINT ( 'NONE',  ( 13.92699808111095905, -7.117895771238833547, -219.6066573659836081 ) ) ;
#16734 = DIRECTION ( 'NONE',  ( -0.000000000000000000, -0.000000000000000000, 1.000000000000000000 ) ) ;
#16735 = AXIS2_PLACEMENT_3D ( 'NONE', #3001, #16862, #6384 ) ;
#16736 = VERTEX_POINT ( 'NONE', #8874 ) ;
#16737 = CARTESIAN_POINT ( 'NONE',  ( -18.09776816382430908, 23.50806826204562583, -229.9568677523880638 ) ) ;
#16738 = CARTESIAN_POINT ( 'NONE',  ( -3.664580975482237157, -26.87662451849047329, -230.7630177344243236 ) ) ;
#16739 = DIRECTION ( 'NONE',  ( 1.000000000000000000, 0.000000000000000000, 0.000000000000000000 ) ) ;
#16740 = CARTESIAN_POINT ( 'NONE',  ( 12.18657022793382794, 26.76558097653315471, -221.8882195427397335 ) ) ;
#16741 = CARTESIAN_POINT ( 'NONE',  ( -1.232595164407830946E-29, 17.50000000000007105, -55.00000000000000000 ) ) ;
#16742 = CARTESIAN_POINT ( 'NONE',  ( 22.36788034568564854, -2.140002702436959225, -217.7104380410378610 ) ) ;
#16743 = CARTESIAN_POINT ( 'NONE',  ( -13.56774755469388616, 7.311522441667196226, -219.1912666243428021 ) ) ;
#16744 = CARTESIAN_POINT ( 'NONE',  ( -16.09559989144903369, 12.31939076846282966, -216.7948290530243298 ) ) ;
#16745 = CARTESIAN_POINT ( 'NONE',  ( 24.78377098693636427, 3.871650763546384155, -231.3521132786341923 ) ) ;
#16746 = CARTESIAN_POINT ( 'NONE',  ( 13.70955873423178772, 0.4527561487833433596, -222.0331215939001197 ) ) ;
#16747 = CARTESIAN_POINT ( 'NONE',  ( 21.91452165549967290, -0.08546329518268500069, -222.0000000000000000 ) ) ;
#16748 = CARTESIAN_POINT ( 'NONE',  ( -14.29986196492902550, 0.06805469746732484282, -227.4167624117703213 ) ) ;
#16749 = CARTESIAN_POINT ( 'NONE',  ( 24.99579664921074240, -7.791002435033769657, -229.1824765006467715 ) ) ;
#16750 = VECTOR ( 'NONE', #3667, 1000.000000000000000 ) ;
#16751 = CARTESIAN_POINT ( 'NONE',  ( -20.85586116824185510, -1.996934699305910499, -232.3804859832740135 ) ) ;
#16752 = CIRCLE ( 'NONE', #12431, 3.000000000000002665 ) ;
#16753 = CARTESIAN_POINT ( 'NONE',  ( 21.13757381859892348, -0.8461838617117842798, -227.8833645607415974 ) ) ;
#16754 = FACE_OUTER_BOUND ( 'NONE', #13379, .T. ) ;
#16755 = CARTESIAN_POINT ( 'NONE',  ( 8.961491954973460849, 17.27041174997091844, -219.7661252763212474 ) ) ;
#16756 = CARTESIAN_POINT ( 'NONE',  ( 3.813635332914135923, -14.61080527247722927, -220.2619188551939828 ) ) ;
#16757 = CARTESIAN_POINT ( 'NONE',  ( 18.00123703865980218, -15.82960056198189491, -233.0014896689109776 ) ) ;
#16758 = CARTESIAN_POINT ( 'NONE',  ( -11.35482716595652875, 11.86850131893102223, -220.6599844941370350 ) ) ;
#16759 = CARTESIAN_POINT ( 'NONE',  ( -16.37512411505367282, 2.406627362596846620, -227.7341547288202719 ) ) ;
#16760 = CARTESIAN_POINT ( 'NONE',  ( 17.51175949430614409, 14.31829016556564937, -218.8195841045835550 ) ) ;
#16761 = ORIENTED_EDGE ( 'NONE', *, *, #586, .F. ) ;
#16762 = CARTESIAN_POINT ( 'NONE',  ( 7.797975340826715396, -14.61189063385648623, -232.7894517818505733 ) ) ;
#16763 = CARTESIAN_POINT ( 'NONE',  ( -14.50000000000000000, 1.775737858763662015E-15, 93.00000000000000000 ) ) ;
#16764 = CARTESIAN_POINT ( 'NONE',  ( -11.80036766549451599, 3.629178540272184783, -221.4826559383200220 ) ) ;
#16765 = CARTESIAN_POINT ( 'NONE',  ( 4.024086222410633518, 12.48004227094270746, -230.0177668608922374 ) ) ;
#16766 = CARTESIAN_POINT ( 'NONE',  ( 4.914880347045685660, 14.54749271951947698, -232.8668677254037789 ) ) ;
#16767 = CARTESIAN_POINT ( 'NONE',  ( 23.10971261601581617, -16.35996695089516706, -224.5402406813554421 ) ) ;
#16768 = CARTESIAN_POINT ( 'NONE',  ( -6.855867220396999251, 12.17758473459128332, -220.6375607554995213 ) ) ;
#16769 = CARTESIAN_POINT ( 'NONE',  ( -14.07917727715460821, 7.534853284453274291, -218.6337090155677458 ) ) ;
#16770 = AXIS2_PLACEMENT_3D ( 'NONE', #13518, #4951, #5059 ) ;
#16771 = CARTESIAN_POINT ( 'NONE',  ( 8.546572992885776543, 19.06776382077057974, -214.7173484156796519 ) ) ;
#16772 = CARTESIAN_POINT ( 'NONE',  ( -22.32700334442577272, 3.978587747811427988, -218.4803616146862453 ) ) ;
#16773 = APPLICATION_CONTEXT ( 'automotive_design' ) ;
#16774 =( GEOMETRIC_REPRESENTATION_CONTEXT ( 3 ) GLOBAL_UNCERTAINTY_ASSIGNED_CONTEXT ( ( #4463 ) ) GLOBAL_UNIT_ASSIGNED_CONTEXT ( ( #10987, #21645, #6016 ) ) REPRESENTATION_CONTEXT ( 'NONE', 'WORKASPACE' ) );
#16775 = CARTESIAN_POINT ( 'NONE',  ( -3.755296588130283553, 23.77975947300719284, -233.7323173085780752 ) ) ;
#16776 = CARTESIAN_POINT ( 'NONE',  ( -5.709328484389660119, 9.211115167980505447, 92.00000000000000000 ) ) ;
#16777 = CARTESIAN_POINT ( 'NONE',  ( 9.253909228257674258, 17.69332415812615977, -230.9900471521432621 ) ) ;
#16778 = CARTESIAN_POINT ( 'NONE',  ( 28.52058947142581502, -1.755848367977142610, -221.9695116608532715 ) ) ;
#16779 = DIRECTION ( 'NONE',  ( -1.000000000000000000, 0.000000000000000000, 0.000000000000000000 ) ) ;
#16780 = PRODUCT ( 'shaft', 'shaft', '', ( #733 ) ) ;
#16781 = CARTESIAN_POINT ( 'NONE',  ( -27.88251101234890328, -7.575382714962081820, -221.6715981084135478 ) ) ;
#16782 = CARTESIAN_POINT ( 'NONE',  ( 27.40550551777678123, 5.967061366481472895, -228.7463788799179554 ) ) ;
#16783 = CARTESIAN_POINT ( 'NONE',  ( -20.23770393675990675, -19.63250941609856426, -227.7987059506201319 ) ) ;
#16784 = DIRECTION ( 'NONE',  ( 0.000000000000000000, 0.000000000000000000, -1.000000000000000000 ) ) ;
#16785 = CARTESIAN_POINT ( 'NONE',  ( -4.080659539198054020, 15.43130099126780408, -228.8058965243247656 ) ) ;
#16786 = CARTESIAN_POINT ( 'NONE',  ( 19.57710422433000019, -21.48596639614413562, -228.6055549924913635 ) ) ;
#16787 = CARTESIAN_POINT ( 'NONE',  ( 8.778334628954494789, 12.71782457734010841, -222.1923057070808909 ) ) ;
#16788 = CARTESIAN_POINT ( 'NONE',  ( -5.775873073292457249, 17.47547275616994256, -218.7209647771908578 ) ) ;
#16789 = CARTESIAN_POINT ( 'NONE',  ( -13.58389614404818069, 15.11490620317918676, -215.3922994348461941 ) ) ;
#16790 = ORIENTED_EDGE ( 'NONE', *, *, #18479, .T. ) ;
#16791 = CARTESIAN_POINT ( 'NONE',  ( -17.12341639776428437, -14.09197680242149886, -218.6048700820433339 ) ) ;
#16792 = CARTESIAN_POINT ( 'NONE',  ( 13.70635042947887428, -1.390919209824193592, -225.3477037409554953 ) ) ;
#16793 = CARTESIAN_POINT ( 'NONE',  ( 0.000000000000000000, 0.000000000000000000, -24.99999999999999645 ) ) ;
#16794 = CARTESIAN_POINT ( 'NONE',  ( -19.19980083083115474, -2.588899828715947038, -216.2953230342753557 ) ) ;
#16795 = CARTESIAN_POINT ( 'NONE',  ( 17.31940731551425827, 24.90170669671083914, -222.9868986272316533 ) ) ;
#16796 = CARTESIAN_POINT ( 'NONE',  ( -17.99155049254074612, 5.190958499132906745, -220.1449419322306937 ) ) ;
#16797 = CARTESIAN_POINT ( 'NONE',  ( 1.682843645364419993, 12.02583837823347679, -224.9288196625490457 ) ) ;
#16798 = CARTESIAN_POINT ( 'NONE',  ( 18.84307465506600465, 4.899879697440840509, -218.2189947030338715 ) ) ;
#16799 = EDGE_LOOP ( 'NONE', ( #6287, #10120, #10740, #5550 ) ) ;
#16800 = CARTESIAN_POINT ( 'NONE',  ( -6.443428446094314310, -19.32516562084312994, -233.2789765400915201 ) ) ;
#16801 = VERTEX_POINT ( 'NONE', #20886 ) ;
#16802 = CARTESIAN_POINT ( 'NONE',  ( -19.43452863239301820, -21.19996443032342626, -221.1427059245750399 ) ) ;
#16803 = CARTESIAN_POINT ( 'NONE',  ( -17.22166590524039265, 4.587137274468266135, -215.4863060638890033 ) ) ;
#16804 = CARTESIAN_POINT ( 'NONE',  ( 7.958080982411646076, -16.12895853103474408, -217.0903302464454612 ) ) ;
#16805 = CARTESIAN_POINT ( 'NONE',  ( 16.48937362995332734, -6.768414299447169213, -233.6525893218997680 ) ) ;
#16806 = CARTESIAN_POINT ( 'NONE',  ( -19.31342342724724759, -3.870051895940637365, -217.8584481481169348 ) ) ;
#16807 = CARTESIAN_POINT ( 'NONE',  ( 18.13412043358480474, 12.55378873098427128, -233.2186159706515696 ) ) ;
#16808 = LINE ( 'NONE', #10282, #5215 ) ;
#16809 = CARTESIAN_POINT ( 'NONE',  ( -12.27164519775873686, 10.97713184439464840, -231.6269036897678291 ) ) ;
#16810 = CARTESIAN_POINT ( 'NONE',  ( 12.11771628698343051, 17.56545729485151952, -218.0322663566023493 ) ) ;
#16811 = CARTESIAN_POINT ( 'NONE',  ( 10.85888002857596923, 15.81835858589122878, -232.3913150909872627 ) ) ;
#16812 = CARTESIAN_POINT ( 'NONE',  ( 6.173705828530630768, 14.85108299334794957, -222.6284669816953112 ) ) ;
#16813 = CARTESIAN_POINT ( 'NONE',  ( 14.85580775603058079, -28.43502054068834894, -222.5810199743787905 ) ) ;
#16814 = CARTESIAN_POINT ( 'NONE',  ( -6.260151855817680300, 29.88549235135308635, -226.8929519981915064 ) ) ;
#16815 = CARTESIAN_POINT ( 'NONE',  ( -20.43618815875133521, 1.403378831510147196, -232.9646741665398224 ) ) ;
#16816 = CARTESIAN_POINT ( 'NONE',  ( 25.52219491023488018, 0.000000000000000000, 89.47905546699919910 ) ) ;
#16817 = CARTESIAN_POINT ( 'NONE',  ( 13.69275646168278371, 8.674223198772375909, -220.8699857572541987 ) ) ;
#16818 = CARTESIAN_POINT ( 'NONE',  ( 6.028509222145709501, -20.27756025184508815, -216.6192952284833950 ) ) ;
#16819 = CARTESIAN_POINT ( 'NONE',  ( -17.78731991475362406, 16.78509880370027929, -218.2387321183659310 ) ) ;
#16820 = CARTESIAN_POINT ( 'NONE',  ( 1.104227501629593045, 25.05528885094460989, -231.9808705443460326 ) ) ;
#16821 = EDGE_CURVE ( 'NONE', #12391, #9851, #15499, .T. ) ;
#16822 = CARTESIAN_POINT ( 'NONE',  ( -12.04756914620937636, -13.80987496524771885, -232.8991007102355582 ) ) ;
#16823 = CARTESIAN_POINT ( 'NONE',  ( 30.52813181070726856, 5.438803974502569361, -223.5441926215666513 ) ) ;
#16824 = CARTESIAN_POINT ( 'NONE',  ( 11.78717493688862206, 28.63884142527983556, -229.7724827508652652 ) ) ;
#16825 = CARTESIAN_POINT ( 'NONE',  ( -6.474151797443945533, 21.29193859232740138, -215.9573456447696458 ) ) ;
#16826 = CARTESIAN_POINT ( 'NONE',  ( 20.29455491689504498, -15.47394441642566143, -219.8812143983372778 ) ) ;
#16827 = CARTESIAN_POINT ( 'NONE',  ( 28.96372477351199137, -10.18960100487436904, -225.5971803650229504 ) ) ;
#16828 = DIRECTION ( 'NONE',  ( -0.000000000000000000, -0.000000000000000000, 1.000000000000000000 ) ) ;
#16829 = CARTESIAN_POINT ( 'NONE',  ( 1.217121169770782663, 15.31158828575123110, -230.6845728599757308 ) ) ;
#16830 = CARTESIAN_POINT ( 'NONE',  ( -10.53630953054794794, -7.637555647514923329, -229.7964863767589918 ) ) ;
#16831 = CARTESIAN_POINT ( 'NONE',  ( 6.589392574981438599, -17.08498810221841069, -232.9613445306918322 ) ) ;
#16832 = B_SPLINE_CURVE_WITH_KNOTS ( 'NONE', 3,
 ( #793, #2700, #1018, #18350, #906, #11154, #16445, #4168, #2808, #17913 ),
 .UNSPECIFIED., .F., .F.,
 ( 4, 2, 2, 2, 4 ),
 ( 0.005560051141765639041, 0.005841872804505881742, 0.006123694467246125310, 0.006405516129986368878, 0.006687337792726613314 ),
 .UNSPECIFIED. ) ;
#16833 = CARTESIAN_POINT ( 'NONE',  ( 13.36656406724190305, -19.73987914515934960, -233.3798509643240209 ) ) ;
#16834 = CARTESIAN_POINT ( 'NONE',  ( -9.746008880186941781, 12.96562886885531896, -220.1990846131056401 ) ) ;
#16835 = EDGE_CURVE ( 'NONE', #5465, #20525, #133, .T. ) ;
#16836 = CARTESIAN_POINT ( 'NONE',  ( 14.66646255503707152, 18.43809875292740230, -219.3480462970252063 ) ) ;
#16837 = CARTESIAN_POINT ( 'NONE',  ( 16.23205080756887853, 0.000000000000000000, 93.00000000000000000 ) ) ;
#16838 = CARTESIAN_POINT ( 'NONE',  ( -26.41026844077819291, 5.012316129610852933, -233.8406020309487872 ) ) ;
#16839 = CARTESIAN_POINT ( 'NONE',  ( -26.61609457609114315, -10.18835510800150779, -222.8381276585760702 ) ) ;
#16840 = VERTEX_POINT ( 'NONE', #2671 ) ;
#16841 = CARTESIAN_POINT ( 'NONE',  ( -17.08384421609436643, 23.56421365837046622, -225.2902702884460666 ) ) ;
#16842 = CARTESIAN_POINT ( 'NONE',  ( 14.69879291197755222, 10.86005690695417236, -216.7815908316746913 ) ) ;
#16843 = CARTESIAN_POINT ( 'NONE',  ( -5.836418080594380164, 30.19240250712089590, -223.8354869487762357 ) ) ;
#16844 = CIRCLE ( 'NONE', #11816, 23.00000000000008882 ) ;
#16845 = CARTESIAN_POINT ( 'NONE',  ( 15.07245478799217686, -4.018468087397350175, -231.0118529037252699 ) ) ;
#16846 = DIRECTION ( 'NONE',  ( -1.000000000000000000, 0.000000000000000000, 0.000000000000000000 ) ) ;
#16847 = ORIENTED_EDGE ( 'NONE', *, *, #6721, .T. ) ;
#16848 = CARTESIAN_POINT ( 'NONE',  ( -25.61997837663875188, 10.01664178086244483, -231.6711741719404074 ) ) ;
#16849 = CARTESIAN_POINT ( 'NONE',  ( -26.48368569639269055, -17.40725828600530534, -221.7871577296580199 ) ) ;
#16850 = CARTESIAN_POINT ( 'NONE',  ( 0.000000000000000000, 0.000000000000000000, 95.00000000000000000 ) ) ;
#16851 = CARTESIAN_POINT ( 'NONE',  ( 10.07175337281514871, 14.76776740066196325, -231.7834566702614723 ) ) ;
#16852 = DIRECTION ( 'NONE',  ( 1.000000000000000000, 0.000000000000000000, 0.000000000000000000 ) ) ;
#16853 = CARTESIAN_POINT ( 'NONE',  ( 13.96958060839473958, -9.488587112651741151, -218.7731372952745232 ) ) ;
#16854 = SHAPE_REPRESENTATION_RELATIONSHIP ( 'NONE' , 'NONE' ,  #3834, #13667 ) ;
#16855 = CARTESIAN_POINT ( 'NONE',  ( -16.74550766701807447, 3.787526820511904813, -217.9802846976114381 ) ) ;
#16856 = CARTESIAN_POINT ( 'NONE',  ( -10.33514150881494942, 13.62639309082336503, -216.9544063991933172 ) ) ;
#16857 = CARTESIAN_POINT ( 'NONE',  ( 27.54521312182184545, 10.10774643363308023, -222.6232199463151744 ) ) ;
#16858 = CARTESIAN_POINT ( 'NONE',  ( -6.749503758482277682, -23.22604375411988187, -218.1095993038993299 ) ) ;
#16859 = FACE_OUTER_BOUND ( 'NONE', #14465, .T. ) ;
#16860 = CARTESIAN_POINT ( 'NONE',  ( 21.31262902390056624, 0.4111834581965390645, -232.0572713672585792 ) ) ;
#16861 = AXIS2_PLACEMENT_3D ( 'NONE', #10787, #19104, #2333 ) ;
#16862 = DIRECTION ( 'NONE',  ( -1.000000000000000000, -6.982962677686272233E-15, 0.000000000000000000 ) ) ;
#16863 = CARTESIAN_POINT ( 'NONE',  ( 27.74277644662361197, -2.671700443591659369, -227.2909148725441355 ) ) ;
#16864 = CARTESIAN_POINT ( 'NONE',  ( 14.83290459615719215, -2.296615622475745688, -226.9301701175285757 ) ) ;
#16865 = CARTESIAN_POINT ( 'NONE',  ( -14.50000000000000000, 1.881795382636152632E-15, 94.00000000000000000 ) ) ;
#16866 = CARTESIAN_POINT ( 'NONE',  ( -22.63401512838748175, 0.000000000000000000, 77.51594804401857175 ) ) ;
#16867 = CARTESIAN_POINT ( 'NONE',  ( 3.755480357635514022, 24.23367984900377436, -231.4105847235276201 ) ) ;
#16868 = CARTESIAN_POINT ( 'NONE',  ( 14.43570356028121893, -19.75277720499002498, -215.7015347705405759 ) ) ;
#16869 = CARTESIAN_POINT ( 'NONE',  ( 14.98777556431132219, -10.10815648641214004, -217.9795565018743844 ) ) ;
#16870 = CARTESIAN_POINT ( 'NONE',  ( -14.69827142695382527, 14.49176359921644597, -217.9600391472806109 ) ) ;
#16871 = CARTESIAN_POINT ( 'NONE',  ( 15.96089671440110713, 1.143943728337336374, -218.3532651118343892 ) ) ;
#16872 = CARTESIAN_POINT ( 'NONE',  ( 14.40184562439531213, 6.414772937171507650, -227.4651811604036595 ) ) ;
#16873 = VERTEX_POINT ( 'NONE', #6273 ) ;
#16874 = CARTESIAN_POINT ( 'NONE',  ( -1.686103422391260764, -28.85289795882446029, -227.6662241409997876 ) ) ;
#16875 = DIRECTION ( 'NONE',  ( -2.891205793294678696E-17, 0.000000000000000000, -1.000000000000000000 ) ) ;
#16876 = CARTESIAN_POINT ( 'NONE',  ( -16.95112677453439431, 10.32962960657076934, -214.9445123409346650 ) ) ;
#16877 = EDGE_LOOP ( 'NONE', ( #3322, #3889, #13688, #6020 ) ) ;
#16878 = CARTESIAN_POINT ( 'NONE',  ( 9.253342549662157523, 15.33540844142859605, -216.2601104504267937 ) ) ;
#16879 = CARTESIAN_POINT ( 'NONE',  ( 12.41447124200992391, -12.24348532208574269, -228.9129928441363973 ) ) ;
#16880 = CARTESIAN_POINT ( 'NONE',  ( 11.13678936984666912, 26.95732789089726111, -228.8350761760834757 ) ) ;
#16881 = CARTESIAN_POINT ( 'NONE',  ( -14.68037037322036475, 3.441677802729143920, -220.1396515630443389 ) ) ;
#16882 = CARTESIAN_POINT ( 'NONE',  ( 19.13589083395335422, 16.69125564174534659, -234.7442498487877174 ) ) ;
#16883 = CARTESIAN_POINT ( 'NONE',  ( -25.94982248293519689, 10.67899231259548287, -221.1273147719203962 ) ) ;
#16884 = CARTESIAN_POINT ( 'NONE',  ( -3.060450601941519189, 13.29454208326677289, -222.0135664617158682 ) ) ;
#16885 = CARTESIAN_POINT ( 'NONE',  ( 20.58703255433590940, 0.4816031003617209372, -231.9427175861361263 ) ) ;
#16886 = CARTESIAN_POINT ( 'NONE',  ( 4.894897393135387631, 18.48819632322109996, -230.2131424875790628 ) ) ;
#16887 = CARTESIAN_POINT ( 'NONE',  ( 20.15756451863428111, -2.090604891399794774, -217.8900786001194945 ) ) ;
#16888 = DIRECTION ( 'NONE',  ( 1.000000000000000000, 0.000000000000000000, 0.000000000000000000 ) ) ;
#16889 = ADVANCED_FACE ( 'NONE', ( #16859 ), #1209, .F. ) ;
#16890 = CARTESIAN_POINT ( 'NONE',  ( -23.00000000000000000, 0.000000000000000000, -69.99999999999998579 ) ) ;
#16891 = CARTESIAN_POINT ( 'NONE',  ( -31.84745724608465522, 5.474219582435353004, -224.7210333253351564 ) ) ;
#16892 = CARTESIAN_POINT ( 'NONE',  ( -23.94935377092574669, -14.34094158514532680, -226.5194954081123342 ) ) ;
#16893 = CARTESIAN_POINT ( 'NONE',  ( 18.83090365933349020, 2.940867245730331980, -225.6043723861373280 ) ) ;
#16894 = CARTESIAN_POINT ( 'NONE',  ( -10.23029362138610843, 26.44342627367518617, -221.6879936327511871 ) ) ;
#16895 = CARTESIAN_POINT ( 'NONE',  ( 5.037691872308702301, -15.96383311541683270, -230.0422288358542460 ) ) ;
#16896 = CARTESIAN_POINT ( 'NONE',  ( 21.46274988498219471, 20.25395488059580984, -223.1777011585387243 ) ) ;
#16897 = CARTESIAN_POINT ( 'NONE',  ( -10.23029362138610843, 26.44342627367518617, -221.6879936327511871 ) ) ;
#16898 = CARTESIAN_POINT ( 'NONE',  ( -23.95129667199961077, 20.99391807043993552, -227.1541646794576081 ) ) ;
#16899 = CARTESIAN_POINT ( 'NONE',  ( 31.97344890504648518, -0.7122400102224841767, -225.1892660388073466 ) ) ;
#16900 = ORIENTED_EDGE ( 'NONE', *, *, #21888, .F. ) ;
#16901 = CARTESIAN_POINT ( 'NONE',  ( 11.87982377808925527, 10.85265283465803421, -229.5027252913499183 ) ) ;
#16902 = CARTESIAN_POINT ( 'NONE',  ( -19.84402263676350131, 8.565754689849573111, -217.6561116767911983 ) ) ;
#16903 = CARTESIAN_POINT ( 'NONE',  ( 29.96674103997387206, 4.060923908484647349, -228.5323681967686298 ) ) ;
#16904 = CARTESIAN_POINT ( 'NONE',  ( 1.526556658859590496E-13, -21.80000000000006111, -78.50000000000000000 ) ) ;
#16905 = CARTESIAN_POINT ( 'NONE',  ( -22.27532461284199528, -3.712691205162892416, -215.8122794664481603 ) ) ;
#16906 = CARTESIAN_POINT ( 'NONE',  ( 6.040050017043670394, 13.67534390435379699, -220.4759402345340504 ) ) ;
#16907 = CARTESIAN_POINT ( 'NONE',  ( -26.64664107080812627, 5.256684826493772000, -228.0533579629717735 ) ) ;
#16908 = CARTESIAN_POINT ( 'NONE',  ( -5.836418080594380164, 30.19240250712089590, -223.8354869487762357 ) ) ;
#16909 = CARTESIAN_POINT ( 'NONE',  ( 27.54521312182184545, 10.10774643363308023, -222.6232199463151744 ) ) ;
#16910 = ORIENTED_EDGE ( 'NONE', *, *, #17351, .T. ) ;
#16911 = CARTESIAN_POINT ( 'NONE',  ( -12.75534255189586652, -28.05386989040209400, -226.4018635127162327 ) ) ;
#16912 = EDGE_LOOP ( 'NONE', ( #20790, #9188, #8974, #20899 ) ) ;
#16913 = CARTESIAN_POINT ( 'NONE',  ( -12.58820391453271093, -22.27128923838312247, -218.3899974299303324 ) ) ;
#16914 = EDGE_CURVE ( 'NONE', #8796, #9103, #3923, .T. ) ;
#16915 = CARTESIAN_POINT ( 'NONE',  ( -20.73319232323294514, 5.144688277016327582, -214.6391322078443977 ) ) ;
#16916 = CARTESIAN_POINT ( 'NONE',  ( 6.589392574981438599, -17.08498810221841069, -232.9613445306918322 ) ) ;
#16917 = CARTESIAN_POINT ( 'NONE',  ( -7.913358619554302642, 16.16796202616373890, -233.0981776325470491 ) ) ;
#16918 = CARTESIAN_POINT ( 'NONE',  ( 15.45838063607522805, -1.173615160199915630, -230.4730353221563917 ) ) ;
#16919 = CARTESIAN_POINT ( 'NONE',  ( -15.58529874627549461, -6.917566422457355202, -219.0138643999995054 ) ) ;
#16920 = CARTESIAN_POINT ( 'NONE',  ( 12.23475091788960434, 6.342242864926500800, -221.9572581868331156 ) ) ;
#16921 = CARTESIAN_POINT ( 'NONE',  ( -1.322875655532295358, 1.500000000000000000, -378.2244600276337678 ) ) ;
#16922 = CARTESIAN_POINT ( 'NONE',  ( -9.734169867326336600, 14.53420431798807755, -231.2442251076483046 ) ) ;
#16923 = CARTESIAN_POINT ( 'NONE',  ( 14.87635807518583775, 11.13002414557121789, -232.1789382499626981 ) ) ;
#16924 = CARTESIAN_POINT ( 'NONE',  ( 15.91295838535984331, 21.88410254487826379, -230.9583961155862823 ) ) ;
#16925 = CARTESIAN_POINT ( 'NONE',  ( 11.35656094503625901, 14.01405796444069018, -230.6944611846958537 ) ) ;
#16926 = CARTESIAN_POINT ( 'NONE',  ( 7.117641012966415381, -28.94820313438933113, -231.4073019955615393 ) ) ;
#16927 = CARTESIAN_POINT ( 'NONE',  ( -9.852301241816233457, 15.10013604187968461, -230.8124578431014697 ) ) ;
#16928 = CARTESIAN_POINT ( 'NONE',  ( -13.11494368899652052, 3.355507568391938200, -225.9121440085824304 ) ) ;
#16929 = LINE ( 'NONE', #1504, #20536 ) ;
#16930 = CARTESIAN_POINT ( 'NONE',  ( 25.18785298611088308, 3.974282393449815931, -218.7636041058819956 ) ) ;
#16931 = CARTESIAN_POINT ( 'NONE',  ( 11.61478720377483675, -14.40087791365289860, -230.4552745109343448 ) ) ;
#16932 = CARTESIAN_POINT ( 'NONE',  ( -26.11114532382342901, 12.73400870066318902, -227.7653936945517046 ) ) ;
#16933 = CARTESIAN_POINT ( 'NONE',  ( 10.03842945413050458, 28.43460431997513638, -225.8374938385031214 ) ) ;
#16934 = CARTESIAN_POINT ( 'NONE',  ( -22.51170993270524789, -14.32174306031543054, -231.7292175355062795 ) ) ;
#16935 = CONTEXT_DEPENDENT_SHAPE_REPRESENTATION ( #12600, #13359 ) ;
#16936 = CARTESIAN_POINT ( 'NONE',  ( -17.72669652144150376, 1.460525322529694581, -220.6883622781615202 ) ) ;
#16937 = CARTESIAN_POINT ( 'NONE',  ( 11.84598249547323690, 10.36127485500543699, -218.5481300776139904 ) ) ;
#16938 = VERTEX_POINT ( 'NONE', #20208 ) ;
#16939 = CARTESIAN_POINT ( 'NONE',  ( 1.773982976645536835, 19.12448993322812285, -233.2315972735944172 ) ) ;
#16940 = CARTESIAN_POINT ( 'NONE',  ( 11.86025528723659050, -11.55469215893994850, -227.5711990284272872 ) ) ;
#16941 = CARTESIAN_POINT ( 'NONE',  ( 13.92699808111095905, -7.117895771238833547, -219.6066573659836081 ) ) ;
#16942 = DIRECTION ( 'NONE',  ( 6.982962677686272233E-15, -1.000000000000000000, 0.000000000000000000 ) ) ;
#16943 = CARTESIAN_POINT ( 'NONE',  ( 5.343558017910363667, 26.29639771561252459, -218.1010331760174665 ) ) ;
#16944 = CARTESIAN_POINT ( 'NONE',  ( -11.72787654052445028, -3.882995534642332824, -226.9210218758430244 ) ) ;
#16945 = CARTESIAN_POINT ( 'NONE',  ( -15.17658589853145479, -26.64966442869902252, -226.8090782225333442 ) ) ;
#16946 = CARTESIAN_POINT ( 'NONE',  ( 12.13827923251525220, -9.172799829723585319, -229.1860353116090891 ) ) ;
#16947 = CARTESIAN_POINT ( 'NONE',  ( -14.60180519431160917, 24.46340507526420893, -221.8423643191928534 ) ) ;
#16948 = CARTESIAN_POINT ( 'NONE',  ( 5.446894657575932719, 15.00061806465251557, -226.4498309983864317 ) ) ;
#16949 = CARTESIAN_POINT ( 'NONE',  ( -20.18153419852512442, 14.25141268122526483, -233.5059133483111964 ) ) ;
#16950 = CARTESIAN_POINT ( 'NONE',  ( -27.40681729237160269, 15.04232492504307572, -225.3323746796125704 ) ) ;
#16951 = CARTESIAN_POINT ( 'NONE',  ( -14.73475970555713310, -4.645830632990214148, -227.0446463473171832 ) ) ;
#16952 = ADVANCED_FACE ( 'NONE', ( #9882 ), #16520, .F. ) ;
#16953 = CARTESIAN_POINT ( 'NONE',  ( -4.386767007475907754, 14.39570986262862107, -223.2690175027443615 ) ) ;
#16954 = CARTESIAN_POINT ( 'NONE',  ( 12.81769551943392393, 4.437328497131001193, -221.7762769673541072 ) ) ;
#16955 = CARTESIAN_POINT ( 'NONE',  ( 18.26039090677515375, 26.14311541888654844, -228.1864986152887127 ) ) ;
#16956 = CARTESIAN_POINT ( 'NONE',  ( 11.20610455198612598, -10.15455062626793037, -220.8168162286965526 ) ) ;
#16957 = DIRECTION ( 'NONE',  ( 1.000000000000000000, 0.000000000000000000, 0.000000000000000000 ) ) ;
#16958 = ORIENTED_EDGE ( 'NONE', *, *, #21201, .T. ) ;
#16959 = CARTESIAN_POINT ( 'NONE',  ( -17.79285498209129202, 9.187865686019035749, -216.3798185811636756 ) ) ;
#16960 = CARTESIAN_POINT ( 'NONE',  ( -9.654146510541638193, -9.431978497097317060, -229.7352898675592314 ) ) ;
#16961 = CARTESIAN_POINT ( 'NONE',  ( -19.00000000000001421, 0.000000000000000000, -224.9999999999999716 ) ) ;
#16962 = CARTESIAN_POINT ( 'NONE',  ( 17.43816562714825125, 15.15720016074785903, -232.3748236813696906 ) ) ;
#16963 = CARTESIAN_POINT ( 'NONE',  ( -3.000000000000030198, 0.000000000000000000, -105.0000000000000142 ) ) ;
#16964 = CARTESIAN_POINT ( 'NONE',  ( 22.44368505003003378, -11.72633196808685163, -232.1179326287041533 ) ) ;
#16965 = CARTESIAN_POINT ( 'NONE',  ( -13.65925618638770800, 3.289586759644148817, -222.1579143493116533 ) ) ;
#16966 = PRODUCT ( 'Removable  Lid', 'Removable  Lid', '', ( #17856 ) ) ;
#16967 = CARTESIAN_POINT ( 'NONE',  ( 16.40130693394614525, -0.1574073183566240264, -221.9481963320051534 ) ) ;
#16968 = CARTESIAN_POINT ( 'NONE',  ( -1.097449620509919788, -25.21235133823365260, -218.6697740411501059 ) ) ;
#16969 = AXIS2_PLACEMENT_3D ( 'NONE', #72, #13815, #20654 ) ;
#16970 = CARTESIAN_POINT ( 'NONE',  ( 0.000000000000000000, 0.000000000000000000, 75.00000000000000000 ) ) ;
#16971 = CARTESIAN_POINT ( 'NONE',  ( 20.89184612657454920, 5.404957034965973683, -232.0952743654565609 ) ) ;
#16972 = CARTESIAN_POINT ( 'NONE',  ( -18.71530386740073126, -0.6857509888707814527, -217.6195632122020527 ) ) ;
#16973 = CARTESIAN_POINT ( 'NONE',  ( 11.03497432892593721, -13.14185978141811972, -229.3300340223075011 ) ) ;
#16974 = CARTESIAN_POINT ( 'NONE',  ( 12.90817018730756516, -2.541983760742972720, -223.3958483567685391 ) ) ;
#16975 = CARTESIAN_POINT ( 'NONE',  ( -23.00000000000000000, -0.6598369341251709708, 10.00000000000000178 ) ) ;
#16976 = CARTESIAN_POINT ( 'NONE',  ( 10.64724148863252395, 12.28344647332184181, -223.6549461381946173 ) ) ;
#16977 = CIRCLE ( 'NONE', #4027, 17.50000000000000711 ) ;
#16978 = CARTESIAN_POINT ( 'NONE',  ( 5.446894657575932719, 15.00061806465251557, -226.4498309983864317 ) ) ;
#16979 = CARTESIAN_POINT ( 'NONE',  ( 9.181101971147782592, -9.127577137574531818, -229.3209091633710273 ) ) ;
#16980 = CARTESIAN_POINT ( 'NONE',  ( 11.39114332821395692, -8.257479203742953189, -226.5648397932267528 ) ) ;
#16981 = ORIENTED_EDGE ( 'NONE', *, *, #4047, .F. ) ;
#16982 = CARTESIAN_POINT ( 'NONE',  ( -20.47640197314466093, 18.50423766437512541, -220.4440130802851456 ) ) ;
#16983 = CARTESIAN_POINT ( 'NONE',  ( -16.27736488614644372, 5.941157768540612949, -228.4237983497913547 ) ) ;
#16984 = CARTESIAN_POINT ( 'NONE',  ( 13.72034832542693827, 10.98995328009155692, -220.6189139471235592 ) ) ;
#16985 = ORIENTED_EDGE ( 'NONE', *, *, #4161, .T. ) ;
#16986 = CARTESIAN_POINT ( 'NONE',  ( -3.821460206879919941, -14.75247343660110921, -225.5705290259156470 ) ) ;
#16987 = CARTESIAN_POINT ( 'NONE',  ( -4.782033626261148029, -9.864562363145054746, 92.00000000000000000 ) ) ;
#16988 = CARTESIAN_POINT ( 'NONE',  ( 22.03647168420945590, 0.3315607655625663064, -232.0572713672586644 ) ) ;
#16989 = ORIENTED_EDGE ( 'NONE', *, *, #12643, .T. ) ;
#16990 = CARTESIAN_POINT ( 'NONE',  ( 15.88965480228581839, 12.37830464553330678, -233.8570207506254235 ) ) ;
#16991 = CARTESIAN_POINT ( 'NONE',  ( 12.68099841568652764, -20.61692530233158394, -230.4218470428317573 ) ) ;
#16992 = CARTESIAN_POINT ( 'NONE',  ( 4.354034006296288339, 14.09944204372416188, -221.2519525881239417 ) ) ;
#16993 = CARTESIAN_POINT ( 'NONE',  ( -16.15126510923403202, -0.4755054218165427615, -219.3066569788202571 ) ) ;
#16994 = AXIS2_PLACEMENT_3D ( 'NONE', #15099, #21935, #18582 ) ;
#16995 = EDGE_CURVE ( 'NONE', #9399, #12912, #19877, .T. ) ;
#16996 = CARTESIAN_POINT ( 'NONE',  ( 25.41781277602550304, 19.49958712797920057, -223.1230538376805441 ) ) ;
#16997 = CARTESIAN_POINT ( 'NONE',  ( -20.84243560023798736, 1.479777185913828230, -230.9766426496277631 ) ) ;
#16998 = EDGE_CURVE ( 'NONE', #8296, #16331, #5153, .T. ) ;
#16999 = CARTESIAN_POINT ( 'NONE',  ( -7.825349071214003693, 24.14595706726266755, -216.5959661901539732 ) ) ;
#17000 = CARTESIAN_POINT ( 'NONE',  ( 16.07305932912010960, 0.9253679043337685872, -229.0409936706996064 ) ) ;
#17001 = CARTESIAN_POINT ( 'NONE',  ( 7.080148886126969465, -28.65852557119563926, -219.9679292432588227 ) ) ;
#17002 = CARTESIAN_POINT ( 'NONE',  ( 27.02029988085337919, -0.4174685747284823112, -230.1188858631967378 ) ) ;
#17003 = DIRECTION ( 'NONE',  ( -0.000000000000000000, -1.000000000000000000, -0.000000000000000000 ) ) ;
#17004 = CARTESIAN_POINT ( 'NONE',  ( -14.37894460687751597, -1.926260335694933268, -225.0161641904981593 ) ) ;
#17005 = CARTESIAN_POINT ( 'NONE',  ( 20.89184612657454920, 5.404957034965973683, -232.0952743654565609 ) ) ;
#17006 = CARTESIAN_POINT ( 'NONE',  ( -19.26019478805205054, -16.72235099301716943, -219.5158537523224993 ) ) ;
#17007 = AXIS2_PLACEMENT_3D ( 'NONE', #2759, #13343, #21548 ) ;
#17008 = DIRECTION ( 'NONE',  ( 0.1736481776669307198, 0.000000000000000000, 0.9848077530122080203 ) ) ;
#17009 = AXIS2_PLACEMENT_3D ( 'NONE', #8204, #22028, #1220 ) ;
#17010 =( LENGTH_UNIT ( ) NAMED_UNIT ( * ) SI_UNIT ( .MILLI., .METRE. ) );
#17011 = CARTESIAN_POINT ( 'NONE',  ( 4.804712767000853368, -14.77773536573586455, -228.5128529893618747 ) ) ;
#17012 = CARTESIAN_POINT ( 'NONE',  ( -21.28183200535960040, 1.085030287403131233, -217.0000000015322712 ) ) ;
#17013 = CARTESIAN_POINT ( 'NONE',  ( -11.08731210905863840, 25.61052584666692766, -228.9953606804266997 ) ) ;
#17014 = CARTESIAN_POINT ( 'NONE',  ( -4.450022810944913587, 12.45400981846350597, -225.2098051417536340 ) ) ;
#17015 = VERTEX_POINT ( 'NONE', #8198 ) ;
#17016 = CARTESIAN_POINT ( 'NONE',  ( 29.01190720243894461, 0.5135883731763817295, -231.9442528450179566 ) ) ;
#17017 = ORIENTED_EDGE ( 'NONE', *, *, #11475, .F. ) ;
#17018 = CARTESIAN_POINT ( 'NONE',  ( 17.43816562714825125, 15.15720016074785903, -232.3748236813696906 ) ) ;
#17019 = CARTESIAN_POINT ( 'NONE',  ( -21.01482965301294925, 6.368220028842532798, -231.7530032521518990 ) ) ;
#17020 = CARTESIAN_POINT ( 'NONE',  ( -20.67624351032310059, -0.8683020119106035217, -219.0957770725675005 ) ) ;
#17021 = DIRECTION ( 'NONE',  ( 1.000000000000000000, 0.000000000000000000, 0.000000000000000000 ) ) ;
#17022 = CARTESIAN_POINT ( 'NONE',  ( 12.08198696763335178, 15.54678077493410981, -216.6084679670902631 ) ) ;
#17023 = CIRCLE ( 'NONE', #1188, 27.49181041625929112 ) ;
#17024 = CARTESIAN_POINT ( 'NONE',  ( -20.21481434941064848, 7.972326285609216967, -230.8475376972877484 ) ) ;
#17025 = AXIS2_PLACEMENT_3D ( 'NONE', #18662, #15503, #7067 ) ;
#17026 = CARTESIAN_POINT ( 'NONE',  ( -0.1452471002967452851, 24.29564289358754081, -234.0861481044164805 ) ) ;
#17027 = CARTESIAN_POINT ( 'NONE',  ( 14.64440749032966593, 2.523901497798496596, -225.4572725674553340 ) ) ;
#17028 = CARTESIAN_POINT ( 'NONE',  ( -13.40300228573463848, -19.05792172404923690, -234.2100255530988306 ) ) ;
#17029 = ORIENTED_EDGE ( 'NONE', *, *, #13312, .F. ) ;
#17030 = CARTESIAN_POINT ( 'NONE',  ( -12.35609710479046441, -10.83622032031252758, -230.4552079900997228 ) ) ;
#17031 = CARTESIAN_POINT ( 'NONE',  ( -14.70339349403010942, -0.4153334646997780544, -217.8790668391084466 ) ) ;
#17032 = CARTESIAN_POINT ( 'NONE',  ( 4.682724365302521896, -22.35092628325669750, -215.9543778044225348 ) ) ;
#17033 = CARTESIAN_POINT ( 'NONE',  ( -3.501680520304516264, 14.31538576447642264, -219.8967178229432307 ) ) ;
#17034 = CARTESIAN_POINT ( 'NONE',  ( 25.70000612522241568, -7.596455516557234944, -216.8500112287931074 ) ) ;
#17035 = CARTESIAN_POINT ( 'NONE',  ( -25.95884575339096401, -1.972114683626720044, -231.2145524501483749 ) ) ;
#17036 = CARTESIAN_POINT ( 'NONE',  ( 13.25330606581809789, 10.40242132629824034, -230.9170765704288044 ) ) ;
#17037 = DIRECTION ( 'NONE',  ( -1.000000000000000000, 1.224646799147353454E-16, 0.000000000000000000 ) ) ;
#17038 = CARTESIAN_POINT ( 'NONE',  ( -16.90193019167508126, 18.45790510038867893, -217.5707532411249758 ) ) ;
#17039 = CARTESIAN_POINT ( 'NONE',  ( 17.98704291748025952, 16.14142602298251461, -217.3684083235702644 ) ) ;
#17040 = CARTESIAN_POINT ( 'NONE',  ( 7.743212835174657194, 11.90778931056080481, -226.0491028376908105 ) ) ;
#17041 = CARTESIAN_POINT ( 'NONE',  ( 15.28499842775873319, 22.98894588155567931, -221.0942409093412095 ) ) ;
#17042 = CARTESIAN_POINT ( 'NONE',  ( 4.248462565232024701, -14.07263755978623188, -232.0081791469470716 ) ) ;
#17043 = CIRCLE ( 'NONE', #1223, 10.00000000000000000 ) ;
#17044 = CARTESIAN_POINT ( 'NONE',  ( -6.388048297418547961, 21.92257289597608150, -233.3290245341164848 ) ) ;
#17045 = CARTESIAN_POINT ( 'NONE',  ( 16.91879448796214191, 0.8271603773820436212, -230.0510230802265710 ) ) ;
#17046 = CARTESIAN_POINT ( 'NONE',  ( 4.150966869518468272, -13.66845483776041092, -221.7292245539943565 ) ) ;
#17047 = CARTESIAN_POINT ( 'NONE',  ( -19.65084584916038324, 18.01805631773661176, -219.5040736310571106 ) ) ;
#17048 = CARTESIAN_POINT ( 'NONE',  ( 2.703362520412529779, 29.60004130108520215, -225.6165589735000481 ) ) ;
#17049 = CARTESIAN_POINT ( 'NONE',  ( -21.52428768452188734, -21.65989873160339840, -225.4304055049964006 ) ) ;
#17050 = CARTESIAN_POINT ( 'NONE',  ( 21.04928763009552384, -0.2309942901367783852, -233.9427286327411366 ) ) ;
#17051 = CARTESIAN_POINT ( 'NONE',  ( 11.41911493375616260, 8.796695304819765582, -229.7440655656592412 ) ) ;
#17052 = ORIENTED_EDGE ( 'NONE', *, *, #12725, .T. ) ;
#17053 = CARTESIAN_POINT ( 'NONE',  ( 14.39473142419577023, 15.98257177912839389, -217.4557725731239373 ) ) ;
#17054 = CARTESIAN_POINT ( 'NONE',  ( 26.09199240421564880, -11.03603815124446186, -222.0211821522591435 ) ) ;
#17055 = CARTESIAN_POINT ( 'NONE',  ( 18.79106389458910442, -5.302521403133691358, -233.5021979784848440 ) ) ;
#17056 = DIRECTION ( 'NONE',  ( -1.000000000000000000, 0.000000000000000000, 0.000000000000000000 ) ) ;
#17057 = TOROIDAL_SURFACE ( 'NONE', #1599, 13.12488928717151637, 3.000000000000000000 ) ;
#17058 = CARTESIAN_POINT ( 'NONE',  ( -3.205260335674071648, 17.52234722004434531, -232.9754319808710363 ) ) ;
#17059 = CARTESIAN_POINT ( 'NONE',  ( -23.85689329484546661, -4.322701801676343436, -216.0188046937498996 ) ) ;
#17060 = CARTESIAN_POINT ( 'NONE',  ( -10.42804209284631156, -14.08702332024887305, -217.7386024361820489 ) ) ;
#17061 = CARTESIAN_POINT ( 'NONE',  ( 11.78320976064766690, -8.193118641535518165, -222.2581747538435479 ) ) ;
#17062 = CARTESIAN_POINT ( 'NONE',  ( -12.67136363292824086, 22.56975222910433843, -219.0840033572168011 ) ) ;
#17063 = CARTESIAN_POINT ( 'NONE',  ( 10.01015180241662605, 20.19019600914695900, -219.1042218506083543 ) ) ;
#17064 = CARTESIAN_POINT ( 'NONE',  ( -21.93900267957129557, 7.862893636934532360, -233.4951761057262161 ) ) ;
#17065 = CARTESIAN_POINT ( 'NONE',  ( -28.99982533490676317, 5.894721259135065949, -231.5937499788843468 ) ) ;
#17066 = CARTESIAN_POINT ( 'NONE',  ( -21.38043581477633026, -15.61850963832630335, -229.1016256230698502 ) ) ;
#17067 = CARTESIAN_POINT ( 'NONE',  ( -12.67219131930435694, 19.52425521811199971, -218.0046184995277372 ) ) ;
#17068 = CARTESIAN_POINT ( 'NONE',  ( 23.21336156720804667, 12.57464006230432574, -232.9346648124233070 ) ) ;
#17069 = CARTESIAN_POINT ( 'NONE',  ( 22.92330650806121639, 19.11387742755395180, -231.6463539987045976 ) ) ;
#17070 = CARTESIAN_POINT ( 'NONE',  ( 24.14841045621385263, -15.62485098017456586, -229.9279278555176518 ) ) ;
#17071 = CARTESIAN_POINT ( 'NONE',  ( 0.000000000000000000, 0.000000000000000000, 75.00000000000000000 ) ) ;
#17072 = VERTEX_POINT ( 'NONE', #6494 ) ;
#17073 = CARTESIAN_POINT ( 'NONE',  ( -1.249406995060579062, 25.48934319316224162, -216.9406480707515072 ) ) ;
#17074 = CARTESIAN_POINT ( 'NONE',  ( -26.26363215285178043, -18.18116807333735352, -227.1727963224598739 ) ) ;
#17075 = DIRECTION ( 'NONE',  ( -0.000000000000000000, -0.000000000000000000, 1.000000000000000000 ) ) ;
#17076 = AXIS2_PLACEMENT_3D ( 'NONE', #18407, #18632, #3194 ) ;
#17077 = CARTESIAN_POINT ( 'NONE',  ( 22.66390650824515873, 11.48342577402021725, -231.3155567808436217 ) ) ;
#17078 = CARTESIAN_POINT ( 'NONE',  ( -21.89482327431018760, 1.733733432562314158, -233.1353281693111796 ) ) ;
#17079 = CARTESIAN_POINT ( 'NONE',  ( 10.99893791904045415, -12.61823049403341201, -218.3266956685045841 ) ) ;
#17080 =( NAMED_UNIT ( * ) SI_UNIT ( $, .STERADIAN. ) SOLID_ANGLE_UNIT ( ) );
#17081 = CARTESIAN_POINT ( 'NONE',  ( -26.58771759052039485, 5.114955214121561511, -218.2823714869195442 ) ) ;
#17082 = CARTESIAN_POINT ( 'NONE',  ( 27.08994772491946890, 9.675875910685000747, -221.3471992134593336 ) ) ;
#17083 = EDGE_CURVE ( 'NONE', #16180, #10560, #488, .T. ) ;
#17084 = CARTESIAN_POINT ( 'NONE',  ( -1.544051355262263225, -15.46116467022245011, -222.0171457641791903 ) ) ;
#17085 = CARTESIAN_POINT ( 'NONE',  ( 0.000000000000000000, 17.50000000000000711, -24.99999999999999645 ) ) ;
#17086 = CARTESIAN_POINT ( 'NONE',  ( 28.02123297569005089, 5.903198806000402143, -227.5759114383273811 ) ) ;
#17087 = CARTESIAN_POINT ( 'NONE',  ( -18.46722752239034193, 0.9784074152395518809, -232.1633353206286188 ) ) ;
#17088 = CARTESIAN_POINT ( 'NONE',  ( 15.36293661829273027, -24.44941682316833464, -223.0188286856611626 ) ) ;
#17089 = CARTESIAN_POINT ( 'NONE',  ( -24.76115377241536208, -2.015397159694146456, -231.8500816169410825 ) ) ;
#17090 = CARTESIAN_POINT ( 'NONE',  ( 19.66316721362375475, -2.213178807039759111, -227.0351927580104814 ) ) ;
#17091 = CARTESIAN_POINT ( 'NONE',  ( 8.312165662451315384, 13.84431584962456974, -225.8109542921768025 ) ) ;
#17092 = CARTESIAN_POINT ( 'NONE',  ( 9.132190541728901323, 17.73033835127231939, -219.5524510795130766 ) ) ;
#17093 = CARTESIAN_POINT ( 'NONE',  ( 11.73142668431994018, -22.53166313379442443, -233.8575593048731491 ) ) ;
#17094 = AXIS2_PLACEMENT_3D ( 'NONE', #20240, #12047, #13629 ) ;
#17095 = CARTESIAN_POINT ( 'NONE',  ( 10.30328786010431052, -20.08430705480546408, -216.1847100135515802 ) ) ;
#17096 = STYLED_ITEM ( 'NONE', ( #18167 ), #21321 ) ;
#17097 = CARTESIAN_POINT ( 'NONE',  ( -12.05423124486310904, 12.38527783110887803, -219.7419643105747014 ) ) ;
#17098 = CARTESIAN_POINT ( 'NONE',  ( -26.87016840655871874, 6.086699737350822481, -222.9228935003981746 ) ) ;
#17099 = CARTESIAN_POINT ( 'NONE',  ( 14.02802030611117878, 3.063901161068346646, -225.6350222114233475 ) ) ;
#17100 = CARTESIAN_POINT ( 'NONE',  ( -13.83311471749147259, -24.17028674860418747, -226.2550113133487173 ) ) ;
#17101 = DIRECTION ( 'NONE',  ( -1.000000000000000000, 0.000000000000000000, 0.000000000000000000 ) ) ;
#17102 = ORIENTED_EDGE ( 'NONE', *, *, #20117, .F. ) ;
#17103 = CARTESIAN_POINT ( 'NONE',  ( 14.64440749032966593, 2.523901497798496596, -225.4572725674553340 ) ) ;
#17104 = CARTESIAN_POINT ( 'NONE',  ( 17.47462908134004422, -13.97354901070533906, -218.8807045398700666 ) ) ;
#17105 = CARTESIAN_POINT ( 'NONE',  ( 13.43170911749896490, 19.07691563292472026, -232.7497845103644636 ) ) ;
#17106 = CARTESIAN_POINT ( 'NONE',  ( -6.101488798441174310, 11.33371047077072369, -225.3616985956418546 ) ) ;
#17107 = CARTESIAN_POINT ( 'NONE',  ( 10.22554538262735413, 24.20440706210576209, -215.6176527921760737 ) ) ;
#17108 = ADVANCED_FACE ( 'NONE', ( #8642 ), #12716, .T. ) ;
#17109 = STYLED_ITEM ( 'NONE', ( #6650 ), #10999 ) ;
#17110 = CARTESIAN_POINT ( 'NONE',  ( -9.747505956077446854, 15.39125695327449783, -233.2799778227147840 ) ) ;
#17111 = CARTESIAN_POINT ( 'NONE',  ( -3.326157069579807946, 13.92020081821418565, -220.5733722327383930 ) ) ;
#17112 = CARTESIAN_POINT ( 'NONE',  ( 21.31262902390056624, 0.4111834581965390645, -232.0572713672585792 ) ) ;
#17113 = CARTESIAN_POINT ( 'NONE',  ( 7.088126259304779353, -19.25156530781288566, -233.7785425911077937 ) ) ;
#17114 = CARTESIAN_POINT ( 'NONE',  ( 24.21331552874348958, 0.07051084380047288602, -231.7986140076958463 ) ) ;
#17115 = DIRECTION ( 'NONE',  ( 1.000000000000000000, 0.000000000000000000, 0.000000000000000000 ) ) ;
#17116 = CARTESIAN_POINT ( 'NONE',  ( -28.55814054826834791, -1.660722980825670048, -228.2640858091212408 ) ) ;
#17117 = CARTESIAN_POINT ( 'NONE',  ( -13.06407726305387307, 3.888674610242962348, -219.0371145420960204 ) ) ;
#17118 = CARTESIAN_POINT ( 'NONE',  ( -13.04844958635619001, -9.307545681632840129, -223.5508123433884009 ) ) ;
#17119 = CARTESIAN_POINT ( 'NONE',  ( 1.304950495335150507, -16.28913491483048759, -229.3926418476436027 ) ) ;
#17120 = EDGE_CURVE ( 'NONE', #3873, #8350, #13936, .T. ) ;
#17121 = CARTESIAN_POINT ( 'NONE',  ( -14.06164063153489252, 2.050767714179807744, -227.2881998904968270 ) ) ;
#17122 = CARTESIAN_POINT ( 'NONE',  ( -3.494873682963683059, 27.70407912598904687, -220.5214894769905243 ) ) ;
#17123 = CARTESIAN_POINT ( 'NONE',  ( -9.350291727197115321, 27.53754332352430367, -230.1504993026967441 ) ) ;
#17124 = ORIENTED_EDGE ( 'NONE', *, *, #464, .F. ) ;
#17125 = CARTESIAN_POINT ( 'NONE',  ( 11.78812147976811175, -1.482036947660514636, -224.5790252820172270 ) ) ;
#17126 = VERTEX_POINT ( 'NONE', #20321 ) ;
#17127 = AXIS2_PLACEMENT_3D ( 'NONE', #7566, #4385, #2376 ) ;
#17128 = CARTESIAN_POINT ( 'NONE',  ( 21.25094435758043332, 17.68230636442804027, -229.7964888993842010 ) ) ;
#17129 = CARTESIAN_POINT ( 'NONE',  ( -21.16281446184100545, 3.810576631694648775, -218.4455094643457187 ) ) ;
#17130 = CARTESIAN_POINT ( 'NONE',  ( -26.91858181626453472, 10.72837452931393187, -223.4556356000267670 ) ) ;
#17131 = CARTESIAN_POINT ( 'NONE',  ( -7.872599071444734697, -12.17161831996831367, -225.5779045487515191 ) ) ;
#17132 = EDGE_CURVE ( 'NONE', #19581, #16287, #4418, .T. ) ;
#17133 = LINE ( 'NONE', #20480, #119 ) ;
#17134 = CARTESIAN_POINT ( 'NONE',  ( 17.23498165643884761, 6.576565757823654934, -216.5785374982484655 ) ) ;
#17135 = CARTESIAN_POINT ( 'NONE',  ( -25.17056316833229701, 11.10725809642625705, -227.0225660235207386 ) ) ;
#17136 = CARTESIAN_POINT ( 'NONE',  ( 11.21112214669106777, 5.418350954422431975, -227.6539796508718325 ) ) ;
#17137 = CARTESIAN_POINT ( 'NONE',  ( 23.04342321161690776, 14.90264581583150694, -218.4777833225197412 ) ) ;
#17138 = CARTESIAN_POINT ( 'NONE',  ( -7.243062456665192883, -20.67674855546218637, -233.5126394780404553 ) ) ;
#17139 = ORIENTED_EDGE ( 'NONE', *, *, #20686, .T. ) ;
#17140 = CARTESIAN_POINT ( 'NONE',  ( -10.73077095140340376, -23.14408218571897891, -231.4559151628563995 ) ) ;
#17141 = CARTESIAN_POINT ( 'NONE',  ( -4.558896566524145655, 13.01459016691503301, -228.3167740496058684 ) ) ;
#17142 = CARTESIAN_POINT ( 'NONE',  ( 3.342529885312644833, -17.78621320651278737, -216.7788622297345853 ) ) ;
#17143 = CARTESIAN_POINT ( 'NONE',  ( 0.9908753270255351575, 13.79205759140780430, -228.0165926715089881 ) ) ;
#17144 = CARTESIAN_POINT ( 'NONE',  ( 24.23593707391374608, -4.329230177290460446, -233.5551557188744312 ) ) ;
#17145 = CARTESIAN_POINT ( 'NONE',  ( -25.42089018817326007, -6.263968923056941307, -218.6542964065910439 ) ) ;
#17146 = CARTESIAN_POINT ( 'NONE',  ( 26.06405806384012536, 5.488112530166501024, -216.5020692413490622 ) ) ;
#17147 = DIRECTION ( 'NONE',  ( 0.000000000000000000, 0.000000000000000000, 1.000000000000000000 ) ) ;
#17148 = CARTESIAN_POINT ( 'NONE',  ( -6.067446494494625142, 16.28408815813367028, -230.0786439517394513 ) ) ;
#17149 = CARTESIAN_POINT ( 'NONE',  ( 15.14859676485869500, 2.119979922547468032, -231.9009926880791284 ) ) ;
#17150 = CARTESIAN_POINT ( 'NONE',  ( 17.97843143658897347, 22.12221935793617078, -220.9346589834416079 ) ) ;
#17151 = CARTESIAN_POINT ( 'NONE',  ( 29.47107563651793427, 6.731311671946880182, -220.0565342412898815 ) ) ;
#17152 = CARTESIAN_POINT ( 'NONE',  ( -1.232290808404003624, -30.06229647885771428, -229.8325228448912583 ) ) ;
#17153 = CARTESIAN_POINT ( 'NONE',  ( 5.434119414999338815, 11.18343085245738777, -221.0450680983404936 ) ) ;
#17154 = PRODUCT ( 'bottom housing_bottom housing', 'bottom housing_bottom housing', '', ( #21532 ) ) ;
#17155 = DIRECTION ( 'NONE',  ( -1.224646799147353207E-16, 1.000000000000000000, 0.000000000000000000 ) ) ;
#17156 = CARTESIAN_POINT ( 'NONE',  ( 7.896007729111394369, -13.22437314876957437, -221.6501328817743683 ) ) ;
#17157 = CARTESIAN_POINT ( 'NONE',  ( -15.30295614572244922, 9.661125001905515930, -218.8475896279880146 ) ) ;
#17158 = CARTESIAN_POINT ( 'NONE',  ( 3.312424284731937618, 15.29837714273186045, -229.5209971419123747 ) ) ;
#17159 = CARTESIAN_POINT ( 'NONE',  ( -16.39524763169126942, -10.97410814576847926, -232.9630882351523837 ) ) ;
#17160 = CARTESIAN_POINT ( 'NONE',  ( 15.39025625686376841, 1.044190007782545226, -218.9203249718910911 ) ) ;
#17161 = CARTESIAN_POINT ( 'NONE',  ( 10.39636392256998221, 18.46527700675686035, -215.1860221565626148 ) ) ;
#17162 = CARTESIAN_POINT ( 'NONE',  ( 8.979547488457603421, 23.24376652602565230, -232.6628827740196357 ) ) ;
#17163 = CARTESIAN_POINT ( 'NONE',  ( 16.48523685932656235, -13.39871719616043855, -218.9387417542926926 ) ) ;
#17164 = CARTESIAN_POINT ( 'NONE',  ( 10.62272209279942992, -9.818939940036045755, -222.1403336352628344 ) ) ;
#17165 = CARTESIAN_POINT ( 'NONE',  ( 13.43170911749896490, 19.07691563292472026, -232.7497845103644636 ) ) ;
#17166 = CARTESIAN_POINT ( 'NONE',  ( -25.41475252190474521, -13.58614899836300260, -217.5872217295323310 ) ) ;
#17167 = CARTESIAN_POINT ( 'NONE',  ( -9.625604265899946554, -19.21123364792547505, -233.9327940972253259 ) ) ;
#17168 = CARTESIAN_POINT ( 'NONE',  ( 12.70477135646371281, -9.814387909761604689, -230.3443492180780652 ) ) ;
#17169 = CARTESIAN_POINT ( 'NONE',  ( -10.46043650402819125, 8.998596506756641134, -222.4402691847174083 ) ) ;
#17170 = CARTESIAN_POINT ( 'NONE',  ( 27.94758519801750296, 7.894658480667867018, -227.3974864124137127 ) ) ;
#17171 = EDGE_CURVE ( 'NONE', #16402, #9939, #4073, .T. ) ;
#17172 = CARTESIAN_POINT ( 'NONE',  ( -14.70651859537745487, 4.211702956367679107, -230.0357207626005334 ) ) ;
#17173 = CARTESIAN_POINT ( 'NONE',  ( -9.734169867326336600, 14.53420431798807755, -231.2442251076483046 ) ) ;
#17174 = CARTESIAN_POINT ( 'NONE',  ( 21.85730963248023428, -9.423385237436111339, -216.6089804361807580 ) ) ;
#17175 = ORIENTED_EDGE ( 'NONE', *, *, #8982, .F. ) ;
#17176 = CARTESIAN_POINT ( 'NONE',  ( -5.775873073292457249, 17.47547275616994256, -218.7209647771908578 ) ) ;
#17177 = CARTESIAN_POINT ( 'NONE',  ( 27.13894094332088969, 12.30518789341946295, -220.2765066586875093 ) ) ;
#17178 = CARTESIAN_POINT ( 'NONE',  ( 10.02118533929671074, 10.65166262057242008, -217.7534731326719566 ) ) ;
#17179 = CARTESIAN_POINT ( 'NONE',  ( 25.90657540470570197, -10.31326923046670885, -218.6707845005603019 ) ) ;
#17180 = DIRECTION ( 'NONE',  ( 0.000000000000000000, 0.000000000000000000, -1.000000000000000000 ) ) ;
#17181 = ORIENTED_EDGE ( 'NONE', *, *, #18365, .T. ) ;
#17182 = CARTESIAN_POINT ( 'NONE',  ( -0.3969026096611234511, 20.89748314411456676, -216.3289738411752978 ) ) ;
#17183 = CARTESIAN_POINT ( 'NONE',  ( -12.58473846644578664, -2.158129970029659006, -220.6199603830026206 ) ) ;
#17184 = DIRECTION ( 'NONE',  ( -1.000000000000000000, 0.000000000000000000, 0.000000000000000000 ) ) ;
#17185 = CARTESIAN_POINT ( 'NONE',  ( 14.85123888640019452, 5.067529763532427012, -221.9058491819374979 ) ) ;
#17186 = CARTESIAN_POINT ( 'NONE',  ( -15.15110768032078070, 3.517015312212880218, -219.5479300368539270 ) ) ;
#17187 = CARTESIAN_POINT ( 'NONE',  ( 25.83609367470520723, -15.13481494965009411, -225.4685613576401124 ) ) ;
#17188 = CARTESIAN_POINT ( 'NONE',  ( -20.94800339253696109, 4.477632454355491731, -216.5423208360950298 ) ) ;
#17189 = CARTESIAN_POINT ( 'NONE',  ( -22.47200958260654957, 4.697452857301940732, -216.5879371680706242 ) ) ;
#17190 = CARTESIAN_POINT ( 'NONE',  ( -5.322766963623397629, -16.65786661440869665, -219.3972027188067671 ) ) ;
#17191 = DIRECTION ( 'NONE',  ( -1.000000000000000000, 0.000000000000000000, -0.000000000000000000 ) ) ;
#17192 = CARTESIAN_POINT ( 'NONE',  ( -21.58783780880416003, 7.944440104776258949, 6.107615235951442401 ) ) ;
#17193 = CARTESIAN_POINT ( 'NONE',  ( -19.25929423112888017, 9.818144317380269825, -216.1837936240308409 ) ) ;
#17194 = CARTESIAN_POINT ( 'NONE',  ( 16.20395612672116314, -10.90071921976151081, -219.5016540749954856 ) ) ;
#17195 = CARTESIAN_POINT ( 'NONE',  ( -28.42127686227592420, -0.6461176296494712812, -221.6028628238154567 ) ) ;
#17196 = EDGE_CURVE ( 'NONE', #2064, #10678, #16662, .T. ) ;
#17197 = CARTESIAN_POINT ( 'NONE',  ( -24.94770155647771048, 1.648570732456370536, 9.868708321403529382 ) ) ;
#17198 = CARTESIAN_POINT ( 'NONE',  ( 16.07044873961816123, 22.39643131523411412, -226.8512752114033901 ) ) ;
#17199 = TOROIDAL_SURFACE ( 'NONE', #10372, 24.63401512838747820, 3.000000000000000888 ) ;
#17200 = CARTESIAN_POINT ( 'NONE',  ( 5.104697752190542559, 17.18208638613223016, -220.3923334988619445 ) ) ;
#17201 = CARTESIAN_POINT ( 'NONE',  ( -3.424405916006480144, -18.03457810294644403, -219.2650390415759318 ) ) ;
#17202 = CARTESIAN_POINT ( 'NONE',  ( 19.88636028791461641, -20.85574262981397453, -219.9907771812986823 ) ) ;
#17203 = ORIENTED_EDGE ( 'NONE', *, *, #13875, .F. ) ;
#17204 = CARTESIAN_POINT ( 'NONE',  ( -18.94992041651601156, 14.87246523864368974, -232.0280096192260828 ) ) ;
#17205 = CARTESIAN_POINT ( 'NONE',  ( -24.82235633397527508, 10.76243500821901300, -227.9886044494091948 ) ) ;
#17206 = CARTESIAN_POINT ( 'NONE',  ( -18.09994298044773942, 1.383435435878707320, -215.7801353739235708 ) ) ;
#17207 = CARTESIAN_POINT ( 'NONE',  ( -2.278185930139247084, -29.13041568434719863, -223.8160414879089046 ) ) ;
#17208 = CARTESIAN_POINT ( 'NONE',  ( -1.259348629394223984, -10.71767081544559375, 91.99999999999998579 ) ) ;
#17209 = ORIENTED_EDGE ( 'NONE', *, *, #1596, .F. ) ;
#17210 = CARTESIAN_POINT ( 'NONE',  ( 25.70381634773192658, 10.55338509461953400, -230.3576492130207782 ) ) ;
#17211 = CARTESIAN_POINT ( 'NONE',  ( 13.43173494629961517, -24.23096015178613172, -223.5315588962966160 ) ) ;
#17212 = CARTESIAN_POINT ( 'NONE',  ( 2.837900457371055563, 25.11342719071438978, -232.9871906064174709 ) ) ;
#17213 = CARTESIAN_POINT ( 'NONE',  ( -22.17339560624464312, 16.26550580028390769, -232.0582861498566274 ) ) ;
#17214 = CIRCLE ( 'NONE', #14343, 23.00000000000000000 ) ;
#17215 = CARTESIAN_POINT ( 'NONE',  ( 10.90540179105271967, 5.382827416078996841, -224.1493061458977820 ) ) ;
#17216 = CARTESIAN_POINT ( 'NONE',  ( 11.13678936984666912, 26.95732789089726111, -228.8350761760834757 ) ) ;
#17217 = CARTESIAN_POINT ( 'NONE',  ( 0.000000000000000000, 0.000000000000000000, -75.00000000000000000 ) ) ;
#17218 = CARTESIAN_POINT ( 'NONE',  ( -1.489322793389167288, -21.37773154815333498, -215.8826219457350817 ) ) ;
#17219 = CARTESIAN_POINT ( 'NONE',  ( 14.98777556431132219, -10.10815648641214004, -217.9795565018743844 ) ) ;
#17220 = CARTESIAN_POINT ( 'NONE',  ( 26.00000000000000000, 0.5000000000000000000, 0.000000000000000000 ) ) ;
#17221 = CARTESIAN_POINT ( 'NONE',  ( -3.400000000000003908, 0.000000000000000000, -224.9999999999999716 ) ) ;
#17222 = CARTESIAN_POINT ( 'NONE',  ( 28.57344184061583192, 5.631897254180425527, -225.1192013637692355 ) ) ;
#17223 = CARTESIAN_POINT ( 'NONE',  ( -13.57658210113775432, -10.11812981318216131, -221.5438341886276987 ) ) ;
#17224 = CARTESIAN_POINT ( 'NONE',  ( 6.250374750423979719, -27.98416211894771521, -222.2453514702945085 ) ) ;
#17225 = CARTESIAN_POINT ( 'NONE',  ( 15.14536540539411114, 2.907144070186200580, -217.8738854795238922 ) ) ;
#17226 = CARTESIAN_POINT ( 'NONE',  ( 9.880827190695510964, 24.82036951119805579, -218.1633337467656020 ) ) ;
#17227 = CARTESIAN_POINT ( 'NONE',  ( -7.352050649209116884, 10.05454564170545417, -223.7370967983176229 ) ) ;
#17228 = EDGE_LOOP ( 'NONE', ( #10087, #4111, #1678, #14346, #11189 ) ) ;
#17229 = CARTESIAN_POINT ( 'NONE',  ( -21.01940116658287749, -3.333607517048045032, -230.8803659671980597 ) ) ;
#17230 = ORIENTED_EDGE ( 'NONE', *, *, #21099, .T. ) ;
#17231 = CARTESIAN_POINT ( 'NONE',  ( 22.02796522526679723, 16.41909032291435366, -220.1590600991317217 ) ) ;
#17232 = EDGE_CURVE ( 'NONE', #12271, #4321, #10913, .T. ) ;
#17233 = CARTESIAN_POINT ( 'NONE',  ( -11.27928845652762213, 14.86256579634383002, -216.2427993537644966 ) ) ;
#17234 = CARTESIAN_POINT ( 'NONE',  ( -15.12838653695630420, 3.161599240781852949, -225.7834014684609656 ) ) ;
#17235 = CARTESIAN_POINT ( 'NONE',  ( -12.35609710479046441, -10.83622032031252758, -230.4552079900997228 ) ) ;
#17236 = CARTESIAN_POINT ( 'NONE',  ( 1.317067778529001989E-13, -19.63401512838747820, -77.51594804401857175 ) ) ;
#17237 = CARTESIAN_POINT ( 'NONE',  ( 27.69955354773053458, 12.81264626165819287, -221.7750850138309602 ) ) ;
#17238 = CARTESIAN_POINT ( 'NONE',  ( -12.01777041390050726, 10.97692933293401474, -227.6853890888168053 ) ) ;
#17239 = CARTESIAN_POINT ( 'NONE',  ( 11.75404126451729070, 5.688294280104953415, -229.3533586468489602 ) ) ;
#17240 = CARTESIAN_POINT ( 'NONE',  ( 14.21126657910812874, 6.833562750302326627, -220.2783117037562874 ) ) ;
#17241 = CARTESIAN_POINT ( 'NONE',  ( -10.76816654174163368, -5.786055782404167402, -221.6662823521482437 ) ) ;
#17242 = ORIENTED_EDGE ( 'NONE', *, *, #16998, .F. ) ;
#17243 = CARTESIAN_POINT ( 'NONE',  ( -7.872599071444734697, -12.17161831996831367, -225.5779045487515191 ) ) ;
#17244 = CARTESIAN_POINT ( 'NONE',  ( -16.89013823391154290, 26.38860451648245231, -225.6449744083545852 ) ) ;
#17245 = CARTESIAN_POINT ( 'NONE',  ( 15.10937218716165020, -26.44221868192832758, -222.7999243300199907 ) ) ;
#17246 = CARTESIAN_POINT ( 'NONE',  ( 1.773982976645536835, 19.12448993322812285, -233.2315972735944172 ) ) ;
#17247 = CARTESIAN_POINT ( 'NONE',  ( 27.54866699188204748, -16.08959018098719085, -223.7550031907416326 ) ) ;
#17248 = DIRECTION ( 'NONE',  ( 0.000000000000000000, 0.000000000000000000, -1.000000000000000000 ) ) ;
#17249 = CARTESIAN_POINT ( 'NONE',  ( -25.44919589272258520, 4.740781954932180575, -232.0725131810460766 ) ) ;
#17250 = DIRECTION ( 'NONE',  ( 0.000000000000000000, 0.000000000000000000, 1.000000000000000000 ) ) ;
#17251 = CARTESIAN_POINT ( 'NONE',  ( -6.407569900110946293, 14.82357759665407215, -221.6203916094852957 ) ) ;
#17252 = CARTESIAN_POINT ( 'NONE',  ( 14.19979467405507556, 6.351366891014061267, -230.8614099669030679 ) ) ;
#17253 = CARTESIAN_POINT ( 'NONE',  ( 15.12287735332712835, 21.03907941686458116, -231.7894952627153202 ) ) ;
#17254 = CARTESIAN_POINT ( 'NONE',  ( 12.89118769162836031, 6.140251663080722899, -228.8792332048833771 ) ) ;
#17255 = CARTESIAN_POINT ( 'NONE',  ( 6.919598145955467849, -31.16410449029495311, -226.5345828574877487 ) ) ;
#17256 = CARTESIAN_POINT ( 'NONE',  ( 10.86206282953156510, 30.27427353967719981, -226.0953027964478110 ) ) ;
#17257 = CARTESIAN_POINT ( 'NONE',  ( 28.57344184061583192, 5.631897254180425527, -225.1192013637692355 ) ) ;
#17258 = CARTESIAN_POINT ( 'NONE',  ( -0.3008257096753846893, -14.77709807386645480, -230.6673697011181048 ) ) ;
#17259 = CARTESIAN_POINT ( 'NONE',  ( -10.32994309255856535, 16.55762392127841665, -218.3313395458419279 ) ) ;
#17260 = CARTESIAN_POINT ( 'NONE',  ( -0.1881941282075867139, 17.37563936270229092, -230.9177995227891813 ) ) ;
#17261 = CARTESIAN_POINT ( 'NONE',  ( -19.31342342724724759, -3.870051895940637365, -217.8584481481169348 ) ) ;
#17262 = CARTESIAN_POINT ( 'NONE',  ( -19.72392517715239535, 13.50888179936880107, -230.7714862421596251 ) ) ;
#17263 = EDGE_CURVE ( 'NONE', #19544, #8365, #1662, .T. ) ;
#17264 = CARTESIAN_POINT ( 'NONE',  ( -19.84402263676350131, 8.565754689849573111, -217.6561116767911983 ) ) ;
#17265 = CARTESIAN_POINT ( 'NONE',  ( 15.46952826979347151, 3.173892190046953665, -221.7237849701489552 ) ) ;
#17266 = EDGE_LOOP ( 'NONE', ( #11997, #20742 ) ) ;
#17267 = CARTESIAN_POINT ( 'NONE',  ( 8.496844655769807630, 14.66037471857024599, -219.1631158796573118 ) ) ;
#17268 = CARTESIAN_POINT ( 'NONE',  ( 14.78595257191855694, -4.705020206487795065, -221.9958499870062099 ) ) ;
#17269 = CARTESIAN_POINT ( 'NONE',  ( 20.28526114930425450, -5.837089636085359245, -233.7994602772149051 ) ) ;
#17270 = CARTESIAN_POINT ( 'NONE',  ( -2.612157044224189484, 27.88031182936952135, -224.5292183073761692 ) ) ;
#17271 = DIRECTION ( 'NONE',  ( 0.000000000000000000, 0.000000000000000000, 1.000000000000000000 ) ) ;
#17272 = CARTESIAN_POINT ( 'NONE',  ( 13.43730899468209294, 8.427513769504761498, -221.4030804848920297 ) ) ;
#17273 = CARTESIAN_POINT ( 'NONE',  ( -13.21307282338718991, -4.958223064515467016, -219.4340824732878730 ) ) ;
#17274 = CARTESIAN_POINT ( 'NONE',  ( -1.643553855084622928, -13.05119293000219294, -222.7191902239112551 ) ) ;
#17275 = CARTESIAN_POINT ( 'NONE',  ( 21.53087031351596892, -21.03550532031109555, -227.1077645633325233 ) ) ;
#17276 = CARTESIAN_POINT ( 'NONE',  ( 2.021807401899061496, 24.17554150923399092, -230.4042646614662146 ) ) ;
#17277 = DIRECTION ( 'NONE',  ( 1.000000000000000000, 0.000000000000000000, 0.000000000000000000 ) ) ;
#17278 = CARTESIAN_POINT ( 'NONE',  ( 14.73597170006453361, 7.272367905564328439, -221.0092474305599239 ) ) ;
#17279 = CARTESIAN_POINT ( 'NONE',  ( -13.98136146596813845, 3.850743984385103680, -228.7620665878280590 ) ) ;
#17280 = CARTESIAN_POINT ( 'NONE',  ( -15.05930145804884290, 24.78193219970826533, -223.0510781988847953 ) ) ;
#17281 = CARTESIAN_POINT ( 'NONE',  ( 28.19769730429874599, -1.268543021275377658, -231.5188709829604363 ) ) ;
#17282 = CARTESIAN_POINT ( 'NONE',  ( 2.630208337444488453, 16.40323635460054774, -219.2570070657488088 ) ) ;
#17283 = CARTESIAN_POINT ( 'NONE',  ( -15.32935061426341861, 5.146212415319166844, -225.5669090095357774 ) ) ;
#17284 = CARTESIAN_POINT ( 'NONE',  ( 7.359401564398577733, 15.81697286067417707, -215.8326977948377987 ) ) ;
#17285 = CARTESIAN_POINT ( 'NONE',  ( 11.64632602964496044, -20.35392056169815689, -232.5450580586399383 ) ) ;
#17286 = CARTESIAN_POINT ( 'NONE',  ( 0.000000000000000000, 0.000000000000000000, -55.00000000000000000 ) ) ;
#17287 = ORIENTED_EDGE ( 'NONE', *, *, #8744, .F. ) ;
#17288 = CARTESIAN_POINT ( 'NONE',  ( -2.735889804569492600, 12.71735652435744512, -225.1194195722198117 ) ) ;
#17289 = CARTESIAN_POINT ( 'NONE',  ( -14.04855893775563125, -7.839533416607601168, -216.6740050463540115 ) ) ;
#17290 = CARTESIAN_POINT ( 'NONE',  ( 0.000000000000000000, 0.000000000000000000, 75.00000000000000000 ) ) ;
#17291 = CARTESIAN_POINT ( 'NONE',  ( 20.23125423326388628, 7.836699765464857137, -217.8891354894872450 ) ) ;
#17292 = CARTESIAN_POINT ( 'NONE',  ( -17.84981083811007707, 0.8485253248287054628, -231.8041300026935119 ) ) ;
#17293 = CARTESIAN_POINT ( 'NONE',  ( 14.98777556431132219, -10.10815648641214004, -217.9795565018743844 ) ) ;
#17294 = SURFACE_SIDE_STYLE ('',( #18977 ) ) ;
#17295 = CARTESIAN_POINT ( 'NONE',  ( -9.716674560061926869, 27.56227806819028103, -219.4917914922789919 ) ) ;
#17296 = CARTESIAN_POINT ( 'NONE',  ( -13.65925618638770800, 3.289586759644148817, -222.1579143493116533 ) ) ;
#17297 = CARTESIAN_POINT ( 'NONE',  ( -4.253447013113726527, -22.64852647464574531, -232.0531923962242615 ) ) ;
#17298 = CARTESIAN_POINT ( 'NONE',  ( -22.56777165119825668, 2.763754931652832307E-15, 90.00000000000000000 ) ) ;
#17299 = CARTESIAN_POINT ( 'NONE',  ( -22.85901762761804079, 2.624492169728419810, 9.672053823688761653 ) ) ;
#17300 = CARTESIAN_POINT ( 'NONE',  ( -26.02440924314744919, 2.824604386891162111, -232.0644005296583430 ) ) ;
#17301 = CARTESIAN_POINT ( 'NONE',  ( 14.02967383842077709, -23.07461891086659378, -219.7428183145782725 ) ) ;
#17302 = CARTESIAN_POINT ( 'NONE',  ( 13.83657615971619848, -1.576202780126219949, -222.4470885262105639 ) ) ;
#17303 = CARTESIAN_POINT ( 'NONE',  ( -23.28342401362511183, 9.104969700446932990, 4.148060178146769417 ) ) ;
#17304 = CARTESIAN_POINT ( 'NONE',  ( 17.02590609996173754, 6.796709046606974169, -230.8496778635019098 ) ) ;
#17305 = CARTESIAN_POINT ( 'NONE',  ( -14.84124724799726991, 21.42277200659090042, -233.6300684249849553 ) ) ;
#17306 = CARTESIAN_POINT ( 'NONE',  ( 14.66646255503707152, 18.43809875292740230, -219.3480462970252063 ) ) ;
#17307 = CARTESIAN_POINT ( 'NONE',  ( -6.114698591673049854, -22.00309638965383030, -231.6969144128436540 ) ) ;
#17308 = CARTESIAN_POINT ( 'NONE',  ( 16.48937362995332734, -6.768414299447169213, -233.6525893218997680 ) ) ;
#17309 = EDGE_LOOP ( 'NONE', ( #1088, #2214, #6436, #11644 ) ) ;
#17310 = ADVANCED_FACE ( 'NONE', ( #22022 ), #2274, .T. ) ;
#17311 = CARTESIAN_POINT ( 'NONE',  ( 3.378648530876271039, 26.08525450992624428, -218.4319906442508454 ) ) ;
#17312 = CARTESIAN_POINT ( 'NONE',  ( -20.21481434941064848, 7.972326285609216967, -230.8475376972877484 ) ) ;
#17313 = CARTESIAN_POINT ( 'NONE',  ( -12.10179538005628963, 1.685214252672075030, -222.4835512146784424 ) ) ;
#17314 = CARTESIAN_POINT ( 'NONE',  ( -14.04666385475200485, -11.54975518965215286, -229.4392169170632201 ) ) ;
#17315 = FACE_OUTER_BOUND ( 'NONE', #5212, .T. ) ;
#17316 = ORIENTED_EDGE ( 'NONE', *, *, #10754, .T. ) ;
#17317 = CARTESIAN_POINT ( 'NONE',  ( 18.84307465506600465, 4.899879697440840509, -218.2189947030338715 ) ) ;
#17318 = CARTESIAN_POINT ( 'NONE',  ( 18.63268865202281432, -19.94522792032704572, -227.6816033052257637 ) ) ;
#17319 = CARTESIAN_POINT ( 'NONE',  ( 7.769483725421269860, 20.68783433326350263, -233.2348178266662728 ) ) ;
#17320 = CARTESIAN_POINT ( 'NONE',  ( -11.98736441306973077, 11.45674391201457176, -217.8252237716743025 ) ) ;
#17321 = AXIS2_PLACEMENT_3D ( 'NONE', #18060, #19626, #11089 ) ;
#17322 = CARTESIAN_POINT ( 'NONE',  ( 16.84354851290083133, 10.42424693870724361, -215.2582953371023109 ) ) ;
#17323 = CIRCLE ( 'NONE', #2564, 3.000000000000002665 ) ;
#17324 = CARTESIAN_POINT ( 'NONE',  ( 10.85888002857596923, 15.81835858589122878, -232.3913150909872627 ) ) ;
#17325 = CARTESIAN_POINT ( 'NONE',  ( -10.71767081544559908, 1.259348629394239083, 92.00000000000002842 ) ) ;
#17326 = CARTESIAN_POINT ( 'NONE',  ( 7.486336813247038258, -29.35413437595724773, -221.4114973598149447 ) ) ;
#17327 = CARTESIAN_POINT ( 'NONE',  ( 21.05631363308661363, -21.50266115212419393, -222.6654548186096747 ) ) ;
#17328 = PLANE ( 'NONE',  #10984 ) ;
#17329 = FACE_OUTER_BOUND ( 'NONE', #8948, .T. ) ;
#17330 = CARTESIAN_POINT ( 'NONE',  ( -15.35982698007958724, 5.508237851081846159, -233.6994028941782631 ) ) ;
#17331 = CARTESIAN_POINT ( 'NONE',  ( -27.59531865868800082, -2.367229732415436771, -222.8128998708299093 ) ) ;
#17332 = CARTESIAN_POINT ( 'NONE',  ( -16.81936022032888545, 5.700806722825413786, -218.5726178058217215 ) ) ;
#17333 = CARTESIAN_POINT ( 'NONE',  ( 1.656472371294090085, 27.29382523973669095, -230.4991099578876117 ) ) ;
#17334 = CARTESIAN_POINT ( 'NONE',  ( 4.238595127209166868, 26.19205419861516404, -230.1142052665570077 ) ) ;
#17335 = ORIENTED_EDGE ( 'NONE', *, *, #17531, .F. ) ;
#17336 = CARTESIAN_POINT ( 'NONE',  ( 31.06375291838557118, -1.327124779900562768, -220.7315133954257647 ) ) ;
#17337 = ORIENTED_EDGE ( 'NONE', *, *, #6998, .T. ) ;
#17338 = CARTESIAN_POINT ( 'NONE',  ( 11.82943521288609823, 27.58963564415041247, -226.1180395413371400 ) ) ;
#17339 = AXIS2_PLACEMENT_3D ( 'NONE', #10358, #2129, #15870 ) ;
#17340 = CARTESIAN_POINT ( 'NONE',  ( -13.48133478602219171, 10.24771958306113362, -218.3822527490931691 ) ) ;
#17341 = CARTESIAN_POINT ( 'NONE',  ( -22.57859951143173660, 16.82392524473188899, -219.5628058978911383 ) ) ;
#17342 = CARTESIAN_POINT ( 'NONE',  ( -24.09642229725868745, -17.04339013636034750, -228.1169379854252384 ) ) ;
#17343 = FACE_OUTER_BOUND ( 'NONE', #19399, .T. ) ;
#17344 = DIRECTION ( 'NONE',  ( 0.000000000000000000, 1.000000000000000000, -0.000000000000000000 ) ) ;
#17345 = CARTESIAN_POINT ( 'NONE',  ( 0.000000000000000000, 19.79999999999999716, 78.50000000000000000 ) ) ;
#17346 = CARTESIAN_POINT ( 'NONE',  ( 13.86459245677513330, 0.7513318449320793846, -221.1689395455950660 ) ) ;
#17347 = CARTESIAN_POINT ( 'NONE',  ( -11.10144104376680652, 18.49675466419975578, -232.2931259015917647 ) ) ;
#17348 = CARTESIAN_POINT ( 'NONE',  ( 18.99256614858759207, 26.22894869843687715, -224.5811130452664202 ) ) ;
#17349 = CARTESIAN_POINT ( 'NONE',  ( -24.68906941503829700, 2.445024713909649705, -232.6803430500543755 ) ) ;
#17350 = CONICAL_SURFACE ( 'NONE', #11597, 23.06814834742187514, 0.2617993877991500740 ) ;
#17351 = EDGE_CURVE ( 'NONE', #16840, #17518, #3353, .T. ) ;
#17352 = CARTESIAN_POINT ( 'NONE',  ( -23.71722460534674681, -17.39027245378339259, -231.9193655574418074 ) ) ;
#17353 = AXIS2_PLACEMENT_3D ( 'NONE', #21802, #15596, #6389 ) ;
#17354 = CARTESIAN_POINT ( 'NONE',  ( -12.88620494227545343, -3.269292211592822461, -225.1464181993036391 ) ) ;
#17355 = CARTESIAN_POINT ( 'NONE',  ( -8.523771322135640816, 24.09653697920728987, -233.1071395647740303 ) ) ;
#17356 = CARTESIAN_POINT ( 'NONE',  ( -12.11864581566431553, -23.10742878804749978, -232.9192999331436909 ) ) ;
#17357 = CARTESIAN_POINT ( 'NONE',  ( -6.282398543089500187, 12.01615879894893801, -228.5121145169883903 ) ) ;
#17358 = CARTESIAN_POINT ( 'NONE',  ( 12.03076347463371398, -25.25364776008588308, -216.5688293904237298 ) ) ;
#17359 = DIRECTION ( 'NONE',  ( -1.000000000000000000, 0.000000000000000000, 0.000000000000000000 ) ) ;
#17360 = CARTESIAN_POINT ( 'NONE',  ( -17.43458823433387650, 2.804998135793385750, -231.8077100320880959 ) ) ;
#17361 = DIRECTION ( 'NONE',  ( -0.000000000000000000, -0.000000000000000000, 1.000000000000000000 ) ) ;
#17362 = CARTESIAN_POINT ( 'NONE',  ( -6.769588938507062004, 18.22485903270490937, -231.3660928915624879 ) ) ;
#17363 = CARTESIAN_POINT ( 'NONE',  ( 25.30228294196351868, 7.987863777258004561, -233.0744943826964573 ) ) ;
#17364 = CARTESIAN_POINT ( 'NONE',  ( 27.04607490430786854, 4.607450003618843049, -220.3758934308003461 ) ) ;
#17365 = CARTESIAN_POINT ( 'NONE',  ( 25.30228294196351868, 7.987863777258004561, -233.0744943826964573 ) ) ;
#17366 = CARTESIAN_POINT ( 'NONE',  ( 4.093437342195941575, -12.31737333437662940, -220.6844603446061512 ) ) ;
#17367 = CARTESIAN_POINT ( 'NONE',  ( 11.13671218404335761, 30.21738803452449673, -224.2405745632392211 ) ) ;
#17368 = TOROIDAL_SURFACE ( 'NONE', #11972, 22.63401512838748175, 3.000000000000002665 ) ;
#17369 = CIRCLE ( 'NONE', #7673, 12.50000000000000355 ) ;
#17370 = CARTESIAN_POINT ( 'NONE',  ( 25.69300549816939494, 5.947472783069708946, -230.6131061331718115 ) ) ;
#17371 = CARTESIAN_POINT ( 'NONE',  ( 0.3839640804239903837, -16.65388496721540790, -217.3312339551772823 ) ) ;
#17372 = CARTESIAN_POINT ( 'NONE',  ( -11.16203726658389606, 26.27101666727781648, -227.8592829514190612 ) ) ;
#17373 = CARTESIAN_POINT ( 'NONE',  ( 18.23116248274160256, 13.99874872632082123, -216.0593560670294835 ) ) ;
#17374 = CARTESIAN_POINT ( 'NONE',  ( -25.95884575339096401, -1.972114683626720044, -231.2145524501483749 ) ) ;
#17375 = CARTESIAN_POINT ( 'NONE',  ( -14.47418542577149836, 8.806675964858893479, -228.0010566307936699 ) ) ;
#17376 = CARTESIAN_POINT ( 'NONE',  ( -0.8357710952364670876, 15.48480697989137234, -216.9118565312697910 ) ) ;
#17377 = CARTESIAN_POINT ( 'NONE',  ( 15.33651282626308010, 7.807290788239344970, -218.6940806506825652 ) ) ;
#17378 = VERTEX_POINT ( 'NONE', #18981 ) ;
#17379 = EDGE_CURVE ( 'NONE', #8742, #17126, #10105, .T. ) ;
#17380 = CARTESIAN_POINT ( 'NONE',  ( 7.513872959756128012, -15.38293111518118295, -221.6143039513618760 ) ) ;
#17381 = ORIENTED_EDGE ( 'NONE', *, *, #7048, .F. ) ;
#17382 = CARTESIAN_POINT ( 'NONE',  ( 9.338484253624125486, -13.53666216847648052, -219.8958652322373837 ) ) ;
#17383 = CARTESIAN_POINT ( 'NONE',  ( -8.791002657293931932, 17.82034842365333205, -218.5247019341474584 ) ) ;
#17384 = VERTEX_POINT ( 'NONE', #12236 ) ;
#17385 = SURFACE_STYLE_FILL_AREA ( #10301 ) ;
#17386 = CARTESIAN_POINT ( 'NONE',  ( 18.23324537670537993, 23.47692953258263771, -224.8333321331434433 ) ) ;
#17387 = CARTESIAN_POINT ( 'NONE',  ( 25.54997870115619207, -2.097555195297153841, -218.7002440566220400 ) ) ;
#17388 = CARTESIAN_POINT ( 'NONE',  ( -0.8413160509385254615, -28.71376977722865931, -218.8117683208458288 ) ) ;
#17389 = AXIS2_PLACEMENT_3D ( 'NONE', #8418, #22135, #9761 ) ;
#17390 = CARTESIAN_POINT ( 'NONE',  ( -1.633632075387274840, -15.48245080501611071, -218.5193615163172751 ) ) ;
#17391 = AXIS2_PLACEMENT_3D ( 'NONE', #4221, #9200, #17752 ) ;
#17392 = CARTESIAN_POINT ( 'NONE',  ( -7.928079932584687128, 26.12067226064367986, -221.2051195461628197 ) ) ;
#17393 = CARTESIAN_POINT ( 'NONE',  ( 1.665334536937734811E-13, -23.00000000000000000, -69.99999999999998579 ) ) ;
#17394 = CARTESIAN_POINT ( 'NONE',  ( 13.72034832542693827, 10.98995328009155692, -220.6189139471235592 ) ) ;
#17395 = CARTESIAN_POINT ( 'NONE',  ( -19.25929423112888017, 9.818144317380269825, -216.1837936240308409 ) ) ;
#17396 = CARTESIAN_POINT ( 'NONE',  ( -6.067446494494625142, 16.28408815813367028, -230.0786439517394513 ) ) ;
#17397 = CARTESIAN_POINT ( 'NONE',  ( 2.893760225568064115, 14.39521026618305477, -227.6654023557511550 ) ) ;
#17398 = CARTESIAN_POINT ( 'NONE',  ( -21.47149190714903710, 3.672831083387290363, -231.0833634068433469 ) ) ;
#17399 = CARTESIAN_POINT ( 'NONE',  ( 9.168912942254459963, 16.03578711007639157, -234.6923200900793347 ) ) ;
#17400 = ADVANCED_FACE ( 'NONE', ( #17418 ), #14869, .T. ) ;
#17401 = CARTESIAN_POINT ( 'NONE',  ( 7.876378987416962296, -12.17572650474792617, -223.4643623724329018 ) ) ;
#17402 = DIRECTION ( 'NONE',  ( 0.000000000000000000, 0.000000000000000000, -1.000000000000000000 ) ) ;
#17403 = ORIENTED_EDGE ( 'NONE', *, *, #20036, .F. ) ;
#17404 = CARTESIAN_POINT ( 'NONE',  ( 0.9046320824004248085, 13.39785254849979701, -226.4815711199935890 ) ) ;
#17405 = ADVANCED_FACE ( 'NONE', ( #18765 ), #1549, .F. ) ;
#17406 = CARTESIAN_POINT ( 'NONE',  ( 18.18465861704851960, -5.084991117879029687, -230.0453011691623999 ) ) ;
#17407 = CARTESIAN_POINT ( 'NONE',  ( 19.06763123184207487, -2.048228142369658666, -218.2337357994572073 ) ) ;
#17408 = CARTESIAN_POINT ( 'NONE',  ( 28.02123297569005089, 5.903198806000402143, -227.5759114383273811 ) ) ;
#17409 = EDGE_CURVE ( 'NONE', #14126, #2304, #18453, .T. ) ;
#17410 = DIRECTION ( 'NONE',  ( 0.000000000000000000, 0.000000000000000000, 1.000000000000000000 ) ) ;
#17411 = CARTESIAN_POINT ( 'NONE',  ( 2.967317674205219191, -16.40215926535219282, -217.6245344443522924 ) ) ;
#17412 = SURFACE_STYLE_USAGE ( .BOTH. , #17294 ) ;
#17413 = CARTESIAN_POINT ( 'NONE',  ( -9.171998067665157350, 9.395241133357435714, -226.3428046914542051 ) ) ;
#17414 = AXIS2_PLACEMENT_3D ( 'NONE', #20074, #1297, #15147 ) ;
#17415 = ORIENTED_EDGE ( 'NONE', *, *, #8228, .F. ) ;
#17416 = CARTESIAN_POINT ( 'NONE',  ( -21.08008464085897060, -0.9048411197481797119, -217.0000000010748522 ) ) ;
#17417 = CARTESIAN_POINT ( 'NONE',  ( -8.465333986790207987, -12.59497810381903982, -228.1424919783533198 ) ) ;
#17418 = FACE_OUTER_BOUND ( 'NONE', #15730, .T. ) ;
#17419 = CARTESIAN_POINT ( 'NONE',  ( -21.95791705875131683, 6.848931874401857023, 7.293650334809576030 ) ) ;
#17420 = CARTESIAN_POINT ( 'NONE',  ( -14.70651859537745487, 4.211702956367679107, -230.0357207626005334 ) ) ;
#17421 = CARTESIAN_POINT ( 'NONE',  ( 20.16749130626988773, -19.72590806003585229, -223.0880382675181579 ) ) ;
#17422 = CARTESIAN_POINT ( 'NONE',  ( 14.88131340536105718, -1.788773220640928807, -222.5905533966261203 ) ) ;
#17423 = CARTESIAN_POINT ( 'NONE',  ( -23.05316956679390472, 9.673225031394522944, 2.619284265031635250 ) ) ;
#17424 = CARTESIAN_POINT ( 'NONE',  ( 13.71585692689473213, 6.523039003617190801, -224.4540437369149402 ) ) ;
#17425 = CARTESIAN_POINT ( 'NONE',  ( -9.722597143579921664, 7.159547510896417499, -227.5730737101346222 ) ) ;
#17426 = CARTESIAN_POINT ( 'NONE',  ( -3.000000000000033751, 0.000000000000000000, -227.9999999999999716 ) ) ;
#17427 = CARTESIAN_POINT ( 'NONE',  ( 12.91443243054181700, 13.28840485332751875, -229.6651346406987955 ) ) ;
#17428 = CARTESIAN_POINT ( 'NONE',  ( -0.6911605129178206575, -19.14003671809244267, -232.0914249810984131 ) ) ;
#17429 = CARTESIAN_POINT ( 'NONE',  ( 15.45838063607522805, -1.173615160199915630, -230.4730353221563917 ) ) ;
#17430 = ORIENTED_EDGE ( 'NONE', *, *, #21540, .F. ) ;
#17431 = CARTESIAN_POINT ( 'NONE',  ( -10.23029362138610843, 26.44342627367518617, -221.6879936327511871 ) ) ;
#17432 = CARTESIAN_POINT ( 'NONE',  ( -22.53796032816233463, 16.84148256071415872, -226.0516062466300582 ) ) ;
#17433 = CARTESIAN_POINT ( 'NONE',  ( -28.99982533490676317, 5.894721259135065949, -231.5937499788843468 ) ) ;
#17434 = AXIS2_PLACEMENT_3D ( 'NONE', #13792, #17271, #8839 ) ;
#17435 = CARTESIAN_POINT ( 'NONE',  ( -15.55375487336196372, -9.676988738288478942, -219.9111427047364202 ) ) ;
#17436 = DIRECTION ( 'NONE',  ( 0.000000000000000000, 0.000000000000000000, 1.000000000000000000 ) ) ;
#17437 = VERTEX_POINT ( 'NONE', #1768 ) ;
#17438 = CARTESIAN_POINT ( 'NONE',  ( 27.54521312182184545, 10.10774643363308023, -222.6232199463151744 ) ) ;
#17439 = CARTESIAN_POINT ( 'NONE',  ( 2.435323595375026073, -28.08909517487921192, -228.1503986837488469 ) ) ;
#17440 = CARTESIAN_POINT ( 'NONE',  ( 19.19288224840068935, 10.13059690604263174, -232.1906135022504998 ) ) ;
#17441 = CARTESIAN_POINT ( 'NONE',  ( -22.04257564474043818, 18.72061943465525857, -219.1781831295219263 ) ) ;
#17442 = CARTESIAN_POINT ( 'NONE',  ( 28.77543668145700195, 2.466904630248945907, -219.6646827587300947 ) ) ;
#17443 = PRODUCT_DEFINITION ( 'UNKNOWN', '', #13550, #13250 ) ;
#17444 = CARTESIAN_POINT ( 'NONE',  ( 4.559463107227270662, 13.27337529356814017, -226.9596205199204633 ) ) ;
#17445 = DIRECTION ( 'NONE',  ( 1.000000000000000000, -0.000000000000000000, -0.000000000000000000 ) ) ;
#17446 = AXIS2_PLACEMENT_3D ( 'NONE', #21574, #7540, #16308 ) ;
#17447 = CARTESIAN_POINT ( 'NONE',  ( -1.177898122437396333, -26.14463525305933445, -216.8677949074964033 ) ) ;
#17448 = CARTESIAN_POINT ( 'NONE',  ( 16.85953475301105442, -7.801609028127129086, -231.9437213283852941 ) ) ;
#17449 = DIRECTION ( 'NONE',  ( 0.000000000000000000, 0.000000000000000000, -1.000000000000000000 ) ) ;
#17450 = DIRECTION ( 'NONE',  ( -0.000000000000000000, -0.000000000000000000, 1.000000000000000000 ) ) ;
#17451 = CARTESIAN_POINT ( 'NONE',  ( -15.42311360645077301, 11.97619046995196079, -234.9244673706848801 ) ) ;
#17452 = CARTESIAN_POINT ( 'NONE',  ( -26.74184309910812374, -3.166857098814535032, -228.4517881524372456 ) ) ;
#17453 = CARTESIAN_POINT ( 'NONE',  ( 19.55931020704464274, 3.833820734573247346, -215.4549349108404783 ) ) ;
#17454 = CARTESIAN_POINT ( 'NONE',  ( 6.040050017043670394, 13.67534390435379699, -220.4759402345340504 ) ) ;
#17455 = CARTESIAN_POINT ( 'NONE',  ( 5.720314275582434327, 25.17872937134267630, -219.7530083620574430 ) ) ;
#17456 = ORIENTED_EDGE ( 'NONE', *, *, #11879, .T. ) ;
#17457 = CARTESIAN_POINT ( 'NONE',  ( 9.097608097968041818, -8.678217757318975600, -221.4288273931462641 ) ) ;
#17458 = ORIENTED_EDGE ( 'NONE', *, *, #16633, .F. ) ;
#17459 = CARTESIAN_POINT ( 'NONE',  ( 14.22574309452842733, 4.476723532073429546, -225.5862451792618231 ) ) ;
#17460 = CARTESIAN_POINT ( 'NONE',  ( -9.747505956077446854, 15.39125695327449783, -233.2799778227147840 ) ) ;
#17461 = CARTESIAN_POINT ( 'NONE',  ( -14.95675039876920032, 11.42095949000369259, -217.2220932760075129 ) ) ;
#17462 = CARTESIAN_POINT ( 'NONE',  ( -9.225692202065292946, -15.38374647092247116, -218.6784895636799320 ) ) ;
#17463 = CARTESIAN_POINT ( 'NONE',  ( -22.04257564474043818, 18.72061943465525857, -219.1781831295219263 ) ) ;
#17464 = FACE_OUTER_BOUND ( 'NONE', #7987, .T. ) ;
#17465 = CIRCLE ( 'NONE', #1273, 17.95451841861686049 ) ;
#17466 = CARTESIAN_POINT ( 'NONE',  ( -14.50000000000000000, 1.775737858763662015E-15, 92.50000000000000000 ) ) ;
#17467 = DIRECTION ( 'NONE',  ( 0.000000000000000000, 0.000000000000000000, 1.000000000000000000 ) ) ;
#17468 = CARTESIAN_POINT ( 'NONE',  ( -9.679547659771646551, 14.60131434979866505, -230.4338124916943968 ) ) ;
#17469 = CARTESIAN_POINT ( 'NONE',  ( 6.550054208186137039, 12.38618022562281595, -231.5087189857719068 ) ) ;
#17470 = CARTESIAN_POINT ( 'NONE',  ( 18.79638869589749461, 0.4878066561304963966, -219.5712168927955759 ) ) ;
#17471 = CARTESIAN_POINT ( 'NONE',  ( -24.34656557913400476, -15.24755813437383267, -217.2726941375463809 ) ) ;
#17472 = CARTESIAN_POINT ( 'NONE',  ( -24.60063047153272819, -17.11178239752603858, -226.7032704813509554 ) ) ;
#17473 = CARTESIAN_POINT ( 'NONE',  ( -7.626320092023432196, 21.25423560278784407, -233.8867968595558295 ) ) ;
#17474 = CARTESIAN_POINT ( 'NONE',  ( -0.6367083786117293531, -29.73461014436635708, -220.1383336929387724 ) ) ;
#17475 = CARTESIAN_POINT ( 'NONE',  ( 15.91295838535984331, 21.88410254487826379, -230.9583961155862823 ) ) ;
#17476 = CARTESIAN_POINT ( 'NONE',  ( 8.727084366397900084, -11.39314604550613375, -218.1375774943401495 ) ) ;
#17477 = CIRCLE ( 'NONE', #11371, 19.63401512838747820 ) ;
#17478 = CARTESIAN_POINT ( 'NONE',  ( -23.00000000000008882, 0.000000000000000000, 75.00000000000000000 ) ) ;
#17479 = EDGE_CURVE ( 'NONE', #8407, #20454, #2994, .T. ) ;
#17480 = CARTESIAN_POINT ( 'NONE',  ( 14.55590852435181226, 2.816890518231522034, -218.5131513550309990 ) ) ;
#17481 = CARTESIAN_POINT ( 'NONE',  ( 2.000000000000000000, 0.000000000000000000, -120.0000000000000142 ) ) ;
#17482 = CARTESIAN_POINT ( 'NONE',  ( -2.426309470044460959, 27.69042070294474556, -223.4541227565655674 ) ) ;
#17483 = CARTESIAN_POINT ( 'NONE',  ( 20.47387447818710271, 7.390772095927000684, -234.0991886097562258 ) ) ;
#17484 = CARTESIAN_POINT ( 'NONE',  ( 14.73698509926073186, 4.443590625350892331, -227.4062002049096236 ) ) ;
#17485 = CARTESIAN_POINT ( 'NONE',  ( 20.18206873099720156, 1.748383523995667987, -234.4526011791959661 ) ) ;
#17486 = CARTESIAN_POINT ( 'NONE',  ( -7.442430984977708164, -13.68264719635657301, -220.8544524341123747 ) ) ;
#17487 = CARTESIAN_POINT ( 'NONE',  ( 1.682843645364419993, 12.02583837823347679, -224.9288196625490457 ) ) ;
#17488 = DIRECTION ( 'NONE',  ( 0.000000000000000000, 0.000000000000000000, 1.000000000000000000 ) ) ;
#17489 = CARTESIAN_POINT ( 'NONE',  ( -3.316277044624852621, -11.89182204942354382, -222.3557635030381618 ) ) ;
#17490 = CARTESIAN_POINT ( 'NONE',  ( -10.29720673141181209, 11.14783905173092649, -222.8560683878917530 ) ) ;
#17491 = AXIS2_PLACEMENT_3D ( 'NONE', #1996, #18693, #3256 ) ;
#17492 = CARTESIAN_POINT ( 'NONE',  ( 11.09231067055629616, 7.417581979752235100, -227.5152062457793534 ) ) ;
#17493 = CARTESIAN_POINT ( 'NONE',  ( -14.48876282330270016, -2.056064607042531911, -223.6537127325441361 ) ) ;
#17494 = CARTESIAN_POINT ( 'NONE',  ( -20.29166677327761903, 16.18344358422343632, -220.0060062064338524 ) ) ;
#17495 = CARTESIAN_POINT ( 'NONE',  ( 1.557078628722260438, 24.20011951319323273, -235.1441088220640268 ) ) ;
#17496 = CARTESIAN_POINT ( 'NONE',  ( 22.05207439088920651, 1.190718621721708947, -218.4927357815377604 ) ) ;
#17497 = ORIENTED_EDGE ( 'NONE', *, *, #5420, .F. ) ;
#17498 = CARTESIAN_POINT ( 'NONE',  ( 7.295492848317381984, -15.02116458630077034, -222.2946426130486941 ) ) ;
#17499 = CARTESIAN_POINT ( 'NONE',  ( 19.33791609681259160, -22.44220124466257360, -223.0821732511882090 ) ) ;
#17500 = CARTESIAN_POINT ( 'NONE',  ( -2.532949683519015949, 17.18298404079579100, -229.0924323441805086 ) ) ;
#17501 = ORIENTED_EDGE ( 'NONE', *, *, #8739, .T. ) ;
#17502 = CARTESIAN_POINT ( 'NONE',  ( 0.000000000000000000, 0.000000000000000000, 75.00000000000000000 ) ) ;
#17503 = CARTESIAN_POINT ( 'NONE',  ( 12.10245006109274080, 26.02147364279441888, -220.6079829738538649 ) ) ;
#17504 = CARTESIAN_POINT ( 'NONE',  ( -29.62561404221338890, 0.9211338879504321620, -221.2478075149841743 ) ) ;
#17505 = CARTESIAN_POINT ( 'NONE',  ( -25.98129645912436914, -15.13773040547512139, -224.1390156429105787 ) ) ;
#17506 = CARTESIAN_POINT ( 'NONE',  ( 6.427665535191954937, -16.40046818492683656, -232.5919299485929912 ) ) ;
#17507 = CARTESIAN_POINT ( 'NONE',  ( -0.7879796667336372851, 21.22375955577181372, -219.1554080315090118 ) ) ;
#17508 = CARTESIAN_POINT ( 'NONE',  ( 12.50000000000000000, 1.530808498934191521E-15, 94.00000000000000000 ) ) ;
#17509 = CARTESIAN_POINT ( 'NONE',  ( 13.17424634425744046, 10.51488364724239588, -221.4616598107521099 ) ) ;
#17510 = CARTESIAN_POINT ( 'NONE',  ( -13.83274569775339202, 16.20364235096346661, -234.0851861771356539 ) ) ;
#17511 = CARTESIAN_POINT ( 'NONE',  ( -3.125843203957122896, 15.99774916147792680, -222.8808123721668721 ) ) ;
#17512 = VERTEX_POINT ( 'NONE', #10438 ) ;
#17513 = CARTESIAN_POINT ( 'NONE',  ( 3.378648530876271039, 26.08525450992624428, -218.4319906442508454 ) ) ;
#17514 = CARTESIAN_POINT ( 'NONE',  ( -16.56270003954679382, 4.935922114544952777, -221.6503923146493378 ) ) ;
#17515 = CARTESIAN_POINT ( 'NONE',  ( 25.70350299105564318, 4.008313962570879241, -233.1578316763087173 ) ) ;
#17516 = CARTESIAN_POINT ( 'NONE',  ( 5.625090746907006611, -14.93184515622287201, -221.0486942310484721 ) ) ;
#17517 = CARTESIAN_POINT ( 'NONE',  ( 24.63401512838748530, 0.000000000000000000, -77.51594804401857175 ) ) ;
#17518 = VERTEX_POINT ( 'NONE', #15292 ) ;
#17519 = EDGE_CURVE ( 'NONE', #5465, #2853, #14511, .T. ) ;
#17520 = CARTESIAN_POINT ( 'NONE',  ( -9.716674560061926869, 27.56227806819028103, -219.4917914922789919 ) ) ;
#17521 = CARTESIAN_POINT ( 'NONE',  ( 20.53331905177824979, -5.913034700419025569, -230.9395893631423462 ) ) ;
#17522 = CARTESIAN_POINT ( 'NONE',  ( 28.52058947142581502, -1.755848367977142610, -221.9695116608532715 ) ) ;
#17523 = CARTESIAN_POINT ( 'NONE',  ( 18.06016678184731461, 2.257982981100609354, -218.9983079406065940 ) ) ;
#17524 = CARTESIAN_POINT ( 'NONE',  ( 1.780803752597676537, -13.83832444325970101, -229.2250779460899537 ) ) ;
#17525 = DIRECTION ( 'NONE',  ( 1.000000000000000000, 0.000000000000000000, 0.000000000000000000 ) ) ;
#17526 = CARTESIAN_POINT ( 'NONE',  ( -18.47334320050258327, 24.79293862780133040, -226.9986786077537317 ) ) ;
#17527 = CARTESIAN_POINT ( 'NONE',  ( -12.99458409358603284, 11.56864380452031504, -232.0274663316965018 ) ) ;
#17528 = CARTESIAN_POINT ( 'NONE',  ( -18.46722752239034193, 0.9784074152395518809, -232.1633353206286188 ) ) ;
#17529 = CARTESIAN_POINT ( 'NONE',  ( -10.95598939193837928, -18.74794674280272488, -217.4432683290776538 ) ) ;
#17530 = CARTESIAN_POINT ( 'NONE',  ( 1.665334536937735820E-13, -23.00000000000006040, 69.99999999999998579 ) ) ;
#17531 = EDGE_CURVE ( 'NONE', #68, #19977, #22042, .T. ) ;
#17532 = CARTESIAN_POINT ( 'NONE',  ( 20.58703255433590940, 0.4816031003617209372, -231.9427175861361263 ) ) ;
#17533 = CARTESIAN_POINT ( 'NONE',  ( -22.04257564474043818, 18.72061943465525857, -219.1781831295219263 ) ) ;
#17534 = CARTESIAN_POINT ( 'NONE',  ( 8.716925653960343467, -14.61958666771473858, -219.5525962724747444 ) ) ;
#17535 = SURFACE_STYLE_USAGE ( .BOTH. , #530 ) ;
#17536 = CARTESIAN_POINT ( 'NONE',  ( 1.387778780781445676E-13, -19.79999999999999716, 78.50000000000000000 ) ) ;
#17537 = CARTESIAN_POINT ( 'NONE',  ( 15.08139719848974103, 12.15862464477973504, -219.3112749338812080 ) ) ;
#17538 = CARTESIAN_POINT ( 'NONE',  ( -14.08083899843152231, 10.81596681319144970, -234.3239311387574446 ) ) ;
#17539 = DIRECTION ( 'NONE',  ( -1.000000000000000000, 0.000000000000000000, 0.000000000000000000 ) ) ;
#17540 = CARTESIAN_POINT ( 'NONE',  ( 21.68053922431529301, 13.05890675940072931, -230.5667798303363440 ) ) ;
#17541 = CARTESIAN_POINT ( 'NONE',  ( 5.517988016436452980, -29.70724229459007759, -226.4438119151823514 ) ) ;
#17542 = ORIENTED_EDGE ( 'NONE', *, *, #2868, .T. ) ;
#17543 = CARTESIAN_POINT ( 'NONE',  ( -0.9249541874382023465, 14.55235618511626328, -223.7321818898853962 ) ) ;
#17544 = CARTESIAN_POINT ( 'NONE',  ( -13.92941769543345032, 11.48925904027772127, -219.8938199480626281 ) ) ;
#17545 = CARTESIAN_POINT ( 'NONE',  ( -14.99655511003079233, 2.316638599135941945, -232.4215266639120046 ) ) ;
#17546 = ORIENTED_EDGE ( 'NONE', *, *, #14512, .F. ) ;
#17547 = CARTESIAN_POINT ( 'NONE',  ( -17.56620462375804692, -17.71942105192161065, -219.9081625180047013 ) ) ;
#17548 = CARTESIAN_POINT ( 'NONE',  ( 2.465190328815661892E-29, 25.00000000000012790, 75.00000000000000000 ) ) ;
#17549 = ORIENTED_EDGE ( 'NONE', *, *, #14990, .F. ) ;
#17550 = CARTESIAN_POINT ( 'NONE',  ( 14.92135368508905202, 7.451356898669101447, -219.1823315336843621 ) ) ;
#17551 = CARTESIAN_POINT ( 'NONE',  ( 4.568467666399979699, -17.52045581048442457, -219.7174082404806938 ) ) ;
#17552 = CARTESIAN_POINT ( 'NONE',  ( 12.71450444683213021, 7.595266944807587350, -224.4213778964231665 ) ) ;
#17553 = CARTESIAN_POINT ( 'NONE',  ( -23.52999999174766543, 19.39566142560855866, -221.9446938626390704 ) ) ;
#17554 = CARTESIAN_POINT ( 'NONE',  ( 25.09997929702755926, 1.294103573351435221, -217.0485712200477906 ) ) ;
#17555 = CARTESIAN_POINT ( 'NONE',  ( 4.389496648589924277, 14.47660514356954131, -220.6151178996808540 ) ) ;
#17556 = DIRECTION ( 'NONE',  ( 1.000000000000000000, -0.000000000000000000, -0.000000000000000000 ) ) ;
#17557 = CARTESIAN_POINT ( 'NONE',  ( -6.512931564893298386, -17.32529878264574563, -216.7284160531958719 ) ) ;
#17558 = CARTESIAN_POINT ( 'NONE',  ( 21.30961698559626427, -20.48616475849644303, -228.5322376518520002 ) ) ;
#17559 = DIRECTION ( 'NONE',  ( 0.000000000000000000, -1.000000000000000000, 0.000000000000000000 ) ) ;
#17560 = DIRECTION ( 'NONE',  ( 1.000000000000000000, 0.000000000000000000, -0.000000000000000000 ) ) ;
#17561 = CARTESIAN_POINT ( 'NONE',  ( -12.13319425917249283, 4.024026700415168634, -229.5243363405849095 ) ) ;
#17562 = CARTESIAN_POINT ( 'NONE',  ( -22.35893676869521229, -6.243268429983856116, -219.2540196962538062 ) ) ;
#17563 = CARTESIAN_POINT ( 'NONE',  ( -12.06153928353927540, 8.661506524875534296, -226.8425068572842349 ) ) ;
#17564 = CARTESIAN_POINT ( 'NONE',  ( -2.692720963948733282, 24.67937284847025481, -218.0912907784291406 ) ) ;
#17565 = CARTESIAN_POINT ( 'NONE',  ( 5.066530254613678785, 15.76189963344335254, -222.1234037505291781 ) ) ;
#17566 = ORIENTED_EDGE ( 'NONE', *, *, #473, .T. ) ;
#17567 = CARTESIAN_POINT ( 'NONE',  ( 18.59830189133340639, -20.05840858737748533, -233.4490516770458157 ) ) ;
#17568 = EDGE_LOOP ( 'NONE', ( #7199, #13616, #7739, #4191 ) ) ;
#17569 = CARTESIAN_POINT ( 'NONE',  ( 14.85123888640019452, 5.067529763532427012, -221.9058491819374979 ) ) ;
#17570 = CARTESIAN_POINT ( 'NONE',  ( -15.23792247720107440, 7.806131751461257373, -230.3336101049160902 ) ) ;
#17571 = CARTESIAN_POINT ( 'NONE',  ( -11.01414002179357610, 8.614420160880040811, -226.3770540798392972 ) ) ;
#17572 = CARTESIAN_POINT ( 'NONE',  ( -13.44605823798860200, -7.860403065310468840, -219.7865185367595586 ) ) ;
#17573 = CARTESIAN_POINT ( 'NONE',  ( -19.00318367631585659, 13.14621133775862916, -233.8403879275295765 ) ) ;
#17574 = AXIS2_PLACEMENT_3D ( 'NONE', #5787, #21421, #21199 ) ;
#17575 = DIRECTION ( 'NONE',  ( 0.000000000000000000, 0.000000000000000000, 1.000000000000000000 ) ) ;
#17576 = CARTESIAN_POINT ( 'NONE',  ( 14.94998080268256757, -2.571697545922924100, -223.4431372107500238 ) ) ;
#17577 = CARTESIAN_POINT ( 'NONE',  ( 25.50289296650958448, 5.998088869914441901, -233.1161630295026157 ) ) ;
#17578 = CARTESIAN_POINT ( 'NONE',  ( -22.03660207690921879, 17.07234836129451949, -222.7335359861421296 ) ) ;
#17579 = CARTESIAN_POINT ( 'NONE',  ( 11.38520239593705163, 18.87760105923376486, -235.3435298574111130 ) ) ;
#17580 = EDGE_CURVE ( 'NONE', #12201, #4564, #12351, .T. ) ;
#17581 = CARTESIAN_POINT ( 'NONE',  ( -16.74550766701807447, 3.787526820511904813, -217.9802846976114381 ) ) ;
#17582 = CARTESIAN_POINT ( 'NONE',  ( -10.39490437715664228, -5.549361993742060406, -223.4983083630424403 ) ) ;
#17583 = CARTESIAN_POINT ( 'NONE',  ( -30.78084016402396372, -2.501288241119758116, -224.5721874330603214 ) ) ;
#17584 = CARTESIAN_POINT ( 'NONE',  ( -8.328662059352005542, 28.53523473722178139, -221.4280032538016201 ) ) ;
#17585 = CARTESIAN_POINT ( 'NONE',  ( -8.379125946468517938, -29.31735857037017468, -221.8060643354269814 ) ) ;
#17586 = CARTESIAN_POINT ( 'NONE',  ( 4.730976410881341465, 17.65764351829336931, -217.6025626048331674 ) ) ;
#17587 = CARTESIAN_POINT ( 'NONE',  ( 10.16297913136807907, -22.49776018550796408, -215.0507767410722977 ) ) ;
#17588 = CARTESIAN_POINT ( 'NONE',  ( -19.80000000000007532, 0.000000000000000000, 78.50000000000000000 ) ) ;
#17589 = CARTESIAN_POINT ( 'NONE',  ( 21.17011458613547248, 1.652544727609948527, -234.6098499860487152 ) ) ;
#17590 = CARTESIAN_POINT ( 'NONE',  ( -3.015877970456246615, 27.27456613555083464, -227.6995284396757313 ) ) ;
#17591 = CARTESIAN_POINT ( 'NONE',  ( 29.47107563651793427, 6.731311671946880182, -220.0565342412898815 ) ) ;
#17592 = CARTESIAN_POINT ( 'NONE',  ( 16.91879448796214191, 0.8271603773820436212, -230.0510230802265710 ) ) ;
#17593 = CARTESIAN_POINT ( 'NONE',  ( 12.54860906168727652, 6.077542143275485031, -228.1605930327268368 ) ) ;
#17594 = CARTESIAN_POINT ( 'NONE',  ( -8.373128421490182660, -27.12459427582015792, -230.7938890564172709 ) ) ;
#17595 = CARTESIAN_POINT ( 'NONE',  ( 5.773563157792669820, 21.63217468058455140, -235.0383461317610170 ) ) ;
#17596 = CARTESIAN_POINT ( 'NONE',  ( 0.000000000000000000, 0.000000000000000000, 75.34729635533385306 ) ) ;
#17597 = CARTESIAN_POINT ( 'NONE',  ( -13.54879968420069503, -27.67624318860520916, -230.2549257473255579 ) ) ;
#17598 = CARTESIAN_POINT ( 'NONE',  ( -4.334015487506815312, 18.19775486192265390, -231.4387392399519285 ) ) ;
#17599 = CARTESIAN_POINT ( 'NONE',  ( 10.88376588832297287, 7.577514201227793400, -222.7215714477710833 ) ) ;
#17600 = CARTESIAN_POINT ( 'NONE',  ( -16.54465188417290022, 6.134005835925411709, -228.8256222654843270 ) ) ;
#17601 = EDGE_CURVE ( 'NONE', #9851, #6126, #526, .T. ) ;
#17602 = CARTESIAN_POINT ( 'NONE',  ( -4.845359737286285551, 16.85396349487340117, -233.9229833851842670 ) ) ;
#17603 = CARTESIAN_POINT ( 'NONE',  ( 25.60482246989237609, 8.614967517510873307, -219.3103232513597618 ) ) ;
#17604 = CARTESIAN_POINT ( 'NONE',  ( 12.66847874168482591, -12.52481328540277161, -229.3043100997535646 ) ) ;
#17605 = ORIENTED_EDGE ( 'NONE', *, *, #65, .T. ) ;
#17606 = CARTESIAN_POINT ( 'NONE',  ( 11.63416633096549369, -11.60453582225250990, -230.7583135875248104 ) ) ;
#17607 = CARTESIAN_POINT ( 'NONE',  ( -3.125843203957122896, 15.99774916147792680, -222.8808123721668721 ) ) ;
#17608 = ORIENTED_EDGE ( 'NONE', *, *, #2239, .F. ) ;
#17609 = DIRECTION ( 'NONE',  ( 0.000000000000000000, 0.000000000000000000, 1.000000000000000000 ) ) ;
#17610 = CARTESIAN_POINT ( 'NONE',  ( 7.743212835174657194, 11.90778931056080481, -226.0491028376908105 ) ) ;
#17611 = CARTESIAN_POINT ( 'NONE',  ( 20.15756451863428111, -2.090604891399794774, -217.8900786001194945 ) ) ;
#17612 = CARTESIAN_POINT ( 'NONE',  ( -13.67406442719345883, -9.319000780081536206, -231.1492214949047934 ) ) ;
#17613 = CARTESIAN_POINT ( 'NONE',  ( 8.332496243628455090, -29.79192972398156769, -226.1452587264855367 ) ) ;
#17614 = CARTESIAN_POINT ( 'NONE',  ( 1.030230143518703345, 18.27887886751213387, -229.5791973322770616 ) ) ;
#17615 = DIRECTION ( 'NONE',  ( -1.000000000000000000, 0.000000000000000000, 0.000000000000000000 ) ) ;
#17616 = CARTESIAN_POINT ( 'NONE',  ( 23.74723497152361062, 5.524508269105988134, -217.6012181427065002 ) ) ;
#17617 = CARTESIAN_POINT ( 'NONE',  ( -9.171998067665157350, 9.395241133357435714, -226.3428046914542051 ) ) ;
#17618 = CARTESIAN_POINT ( 'NONE',  ( -8.308618357598591686, 12.44656112581930785, -228.0014162119141474 ) ) ;
#17619 = EDGE_LOOP ( 'NONE', ( #4884, #5435, #2987, #17337, #8768, #17549 ) ) ;
#17620 = CARTESIAN_POINT ( 'NONE',  ( -2.435715273212520238, 23.41098772907853132, -217.6796576669356966 ) ) ;
#17621 = CARTESIAN_POINT ( 'NONE',  ( 15.96089671440110713, 1.143943728337336374, -218.3532651118343892 ) ) ;
#17622 = CARTESIAN_POINT ( 'NONE',  ( 13.40064012097826307, 2.532414129335418096, -221.5952957478750989 ) ) ;
#17623 = CARTESIAN_POINT ( 'NONE',  ( 18.03651828442428595, -19.10816016050398147, -231.7458924702002037 ) ) ;
#17624 = CARTESIAN_POINT ( 'NONE',  ( 0.000000000000000000, 25.00000000000000000, 75.00000000000000000 ) ) ;
#17625 = ORIENTED_EDGE ( 'NONE', *, *, #4400, .F. ) ;
#17626 = CARTESIAN_POINT ( 'NONE',  ( 11.67669251569587985, 24.04736029062789981, -218.5856804285192254 ) ) ;
#17627 = CARTESIAN_POINT ( 'NONE',  ( 26.42227051273691885, -8.869064526452445918, -225.3570890864022260 ) ) ;
#17628 = DIRECTION ( 'NONE',  ( 1.000000000000000000, 0.000000000000000000, 0.000000000000000000 ) ) ;
#17629 = CARTESIAN_POINT ( 'NONE',  ( 16.07305932912010960, 0.9253679043337685872, -229.0409936706996064 ) ) ;
#17630 = CARTESIAN_POINT ( 'NONE',  ( 1.292981098121811279, -26.53499626907933262, -232.9055005154886828 ) ) ;
#17631 = CARTESIAN_POINT ( 'NONE',  ( -12.90983082593748676, 14.84936372681532823, -233.8009687022269532 ) ) ;
#17632 = CARTESIAN_POINT ( 'NONE',  ( -10.01410430826631170, 16.10970239316000630, -233.6135099156378203 ) ) ;
#17633 = ORIENTED_EDGE ( 'NONE', *, *, #21888, .T. ) ;
#17634 = CARTESIAN_POINT ( 'NONE',  ( -20.26851768784797869, -0.8260594303982465858, -217.1279713726092098 ) ) ;
#17635 = CARTESIAN_POINT ( 'NONE',  ( -15.28220591200235390, -15.65475725988279443, -217.1155325995422913 ) ) ;
#17636 = CARTESIAN_POINT ( 'NONE',  ( -24.79104265374166260, -3.241215102701672457, -9.465926045374253306 ) ) ;
#17637 = CARTESIAN_POINT ( 'NONE',  ( -22.96438540778823878, 1.321627609350921384, 9.917856572734910614 ) ) ;
#17638 = CARTESIAN_POINT ( 'NONE',  ( -11.46843428684449151, 6.508406145394057596, -225.7212143570321814 ) ) ;
#17639 = CARTESIAN_POINT ( 'NONE',  ( 0.09627406729119250550, -13.23594471221713142, -227.7621942207877339 ) ) ;
#17641 = EDGE_CURVE ( 'NONE', #13811, #21551, #14274, .T. ) ;
#17640 = CARTESIAN_POINT ( 'NONE',  ( 14.96415947227435339, -1.927366939720012606, -222.7010313878448358 ) ) ;
#17642 = LINE ( 'NONE', #5358, #11613 ) ;
#17643 = CARTESIAN_POINT ( 'NONE',  ( 21.07144422417032104, 18.33581350331571969, -223.6711752364813890 ) ) ;
#17644 = CARTESIAN_POINT ( 'NONE',  ( -9.045741320599788082, 11.46901338045063312, -219.0588111342715365 ) ) ;
#17645 = CARTESIAN_POINT ( 'NONE',  ( -1.322875655532295136, 1.500000000000000000, -105.0000000000000142 ) ) ;
#17646 = CARTESIAN_POINT ( 'NONE',  ( 18.30590144060498403, 15.06309558287673767, -219.0459394567220102 ) ) ;
#17647 = CARTESIAN_POINT ( 'NONE',  ( 5.319567441806261066, -29.83260615907786573, -224.9444841741296841 ) ) ;
#17648 = CIRCLE ( 'NONE', #9785, 3.000000000000002665 ) ;
#17649 = ORIENTED_EDGE ( 'NONE', *, *, #464, .T. ) ;
#17650 = CARTESIAN_POINT ( 'NONE',  ( -2.692720963948733282, 24.67937284847025481, -218.0912907784291406 ) ) ;
#17651 = CARTESIAN_POINT ( 'NONE',  ( -10.24168223636446662, 16.14271751156598356, -231.4847994864913971 ) ) ;
#17652 = CARTESIAN_POINT ( 'NONE',  ( 18.39384604806649648, 2.566915855367216004, -231.7421336352533103 ) ) ;
#17653 = CARTESIAN_POINT ( 'NONE',  ( -16.76407561856198214, -10.47882714055132070, -219.0733374248486598 ) ) ;
#17654 = DIRECTION ( 'NONE',  ( -1.000000000000000000, 0.000000000000000000, 0.000000000000000000 ) ) ;
#17655 = EDGE_LOOP ( 'NONE', ( #15811, #298 ) ) ;
#17656 = CARTESIAN_POINT ( 'NONE',  ( -21.08008464085897060, -0.9048411197481797119, -217.0000000010748522 ) ) ;
#17657 = CARTESIAN_POINT ( 'NONE',  ( 0.8935217740153370558, -25.09083646304939919, -218.5222943608621335 ) ) ;
#17658 = CARTESIAN_POINT ( 'NONE',  ( 14.95414693437772868, 8.262206471704862665, -230.1862972580043163 ) ) ;
#17659 = CARTESIAN_POINT ( 'NONE',  ( -3.673551555920188783, 29.81207051619892923, -228.8770490300152005 ) ) ;
#17660 = CARTESIAN_POINT ( 'NONE',  ( 17.85905871012913693, 8.463974683125162102, -234.6532732619751300 ) ) ;
#17661 = CARTESIAN_POINT ( 'NONE',  ( 4.883314309504700468, 19.06839645569368358, -217.0171359871271193 ) ) ;
#17662 = CARTESIAN_POINT ( 'NONE',  ( -9.864562363145052970, 4.782033626261182668, 92.00000000000000000 ) ) ;
#17663 = CARTESIAN_POINT ( 'NONE',  ( -13.60146639818222702, -25.11808310587244009, -230.9974232610874196 ) ) ;
#17664 = CARTESIAN_POINT ( 'NONE',  ( 13.28406271702445274, -5.237238614233280742, -225.2640488721434622 ) ) ;
#17665 = FACE_OUTER_BOUND ( 'NONE', #14711, .T. ) ;
#17666 = DIRECTION ( 'NONE',  ( 0.000000000000000000, 0.000000000000000000, 1.000000000000000000 ) ) ;
#17667 = CARTESIAN_POINT ( 'NONE',  ( -28.76901170826145560, 13.32870333992657663, -228.6722616467874616 ) ) ;
#17668 = CARTESIAN_POINT ( 'NONE',  ( -16.42300678490213883, -6.478264502461970054, -228.9348778629521064 ) ) ;
#17669 = CARTESIAN_POINT ( 'NONE',  ( -11.94782396647286049, 8.456988817430419303, -225.5094493096559063 ) ) ;
#17670 = CARTESIAN_POINT ( 'NONE',  ( 14.60728983664449387, 19.38727400458104455, -216.6381802409380555 ) ) ;
#17671 = CARTESIAN_POINT ( 'NONE',  ( 5.646952844456516019, 23.06006924884521325, -218.8221376988549878 ) ) ;
#17672 = ORIENTED_EDGE ( 'NONE', *, *, #8783, .T. ) ;
#17673 = CARTESIAN_POINT ( 'NONE',  ( 25.69865375807269459, -17.81673768310515626, -220.5381737609034474 ) ) ;
#17674 = ORIENTED_EDGE ( 'NONE', *, *, #5134, .T. ) ;
#17675 = CARTESIAN_POINT ( 'NONE',  ( 17.07668571305246985, 2.037405138410691485, -219.7626854147787867 ) ) ;
#17676 = AXIS2_PLACEMENT_3D ( 'NONE', #10979, #17850, #1059 ) ;
#17677 = CARTESIAN_POINT ( 'NONE',  ( -13.24620988741752825, 28.78239319002125285, -225.3527830703614256 ) ) ;
#17678 = CARTESIAN_POINT ( 'NONE',  ( -11.40916210110096962, 20.01996232974788725, -234.3205435716851923 ) ) ;
#17679 = CARTESIAN_POINT ( 'NONE',  ( -28.09913862414779473, -9.456046895945956265, -221.0065986266286870 ) ) ;
#17680 = EDGE_CURVE ( 'NONE', #20147, #20901, #14162, .T. ) ;
#17681 = CARTESIAN_POINT ( 'NONE',  ( -11.79584727357715934, 6.509288465425584036, -222.6080315736180921 ) ) ;
#17682 = CYLINDRICAL_SURFACE ( 'NONE', #20172, 17.50000000000007816 ) ;
#17683 = EDGE_CURVE ( 'NONE', #3040, #16402, #17369, .T. ) ;
#17684 = CARTESIAN_POINT ( 'NONE',  ( 28.78651053433536333, -0.9604905981993369091, -227.3547688931310233 ) ) ;
#17685 = CIRCLE ( 'NONE', #21611, 21.00000000000000000 ) ;
#17686 = CARTESIAN_POINT ( 'NONE',  ( -13.58070052954164275, 11.19572749768420650, -220.2511552028196604 ) ) ;
#17687 = CARTESIAN_POINT ( 'NONE',  ( 14.95834318372430083, -1.617016552789838801, -229.6306532055809271 ) ) ;
#17688 = CARTESIAN_POINT ( 'NONE',  ( -22.47200958260654957, 4.697452857301940732, -216.5879371680706242 ) ) ;
#17689 = CARTESIAN_POINT ( 'NONE',  ( 9.107417252317809186, 16.30291009569977234, -218.0131178633739921 ) ) ;
#17690 = CIRCLE ( 'NONE', #13744, 3.000000000000002665 ) ;
#17691 = CARTESIAN_POINT ( 'NONE',  ( -26.47652094774193188, -8.527600130219385122, -218.5932275281782324 ) ) ;
#17692 = CARTESIAN_POINT ( 'NONE',  ( -0.4548635697939061306, 27.30478022265488036, -219.8474162243132071 ) ) ;
#17693 = CARTESIAN_POINT ( 'NONE',  ( -6.642805165258356404, -28.12267032419628521, -230.9452027245340560 ) ) ;
#17694 = CARTESIAN_POINT ( 'NONE',  ( 5.331555957413248059, 27.50712867803999728, -219.0801070358024276 ) ) ;
#17695 = CARTESIAN_POINT ( 'NONE',  ( 13.52447848812844100, -22.07588418332509050, -234.6412735253872484 ) ) ;
#17696 = CARTESIAN_POINT ( 'NONE',  ( 14.73484710815641030, -0.3083309717192121435, -227.9841133479512223 ) ) ;
#17697 = CARTESIAN_POINT ( 'NONE',  ( -12.33203608746942237, 8.428128317385924717, -222.9277009507565026 ) ) ;
#17698 = DIRECTION ( 'NONE',  ( 1.000000000000000000, 0.000000000000000000, 0.000000000000000000 ) ) ;
#17699 = CARTESIAN_POINT ( 'NONE',  ( 29.82766783012230505, -1.714217446056379934, -229.3564438616236316 ) ) ;
#17700 = CARTESIAN_POINT ( 'NONE',  ( 3.786538429322381383, 16.06208591393598084, -226.9891439814428793 ) ) ;
#17701 = CARTESIAN_POINT ( 'NONE',  ( -12.62195384480319582, 9.244619650382723819, -228.6283004876635516 ) ) ;
#17702 = AXIS2_PLACEMENT_3D ( 'NONE', #22261, #16875, #17101 ) ;
#17703 = CARTESIAN_POINT ( 'NONE',  ( 25.18785298611088308, 3.974282393449815931, -218.7636041058819956 ) ) ;
#17704 = CARTESIAN_POINT ( 'NONE',  ( -10.37556110177195023, -11.10057404503678846, -224.0577835142470349 ) ) ;
#17705 = EDGE_CURVE ( 'NONE', #18856, #7596, #14378, .T. ) ;
#17706 = CARTESIAN_POINT ( 'NONE',  ( 12.08790845148079640, 6.355304031620478078, -220.0087475230167229 ) ) ;
#17707 = DIRECTION ( 'NONE',  ( -0.000000000000000000, -0.000000000000000000, 1.000000000000000000 ) ) ;
#17708 = CARTESIAN_POINT ( 'NONE',  ( -5.787689185779406387, -30.68964578337966387, -228.1462806397894383 ) ) ;
#17709 = CARTESIAN_POINT ( 'NONE',  ( -10.16319438574952372, 11.71174522937666040, -227.8434026503654479 ) ) ;
#17710 = AXIS2_PLACEMENT_3D ( 'NONE', #10397, #5203, #12086 ) ;
#17711 = CARTESIAN_POINT ( 'NONE',  ( 15.88043104796248528, 11.88135572392608807, -216.2525917828042168 ) ) ;
#17712 = AXIS2_PLACEMENT_3D ( 'NONE', #13040, #17784, #2565 ) ;
#17713 = CARTESIAN_POINT ( 'NONE',  ( -14.59766675578715223, 7.926254675926275972, -222.3706877972550444 ) ) ;
#17714 = CARTESIAN_POINT ( 'NONE',  ( 4.754245974719506940, 31.05377813473586102, -220.6166503949300193 ) ) ;
#17715 = CARTESIAN_POINT ( 'NONE',  ( 27.16757474806794903, 2.676291341565463888, -220.8863403533574115 ) ) ;
#17716 = ORIENTED_EDGE ( 'NONE', *, *, #17409, .F. ) ;
#17717 = CARTESIAN_POINT ( 'NONE',  ( 18.63268865202281432, -19.94522792032704572, -227.6816033052257637 ) ) ;
#17718 = CARTESIAN_POINT ( 'NONE',  ( 8.767697218519710844, -14.65932909790238448, -230.8495237012982386 ) ) ;
#17719 = CARTESIAN_POINT ( 'NONE',  ( -3.389634396460917465, 16.42708991135657115, -221.9057377485790994 ) ) ;
#17720 = DIRECTION ( 'NONE',  ( -1.000000000000000000, 0.000000000000000000, 0.000000000000000000 ) ) ;
#17721 = CARTESIAN_POINT ( 'NONE',  ( 19.20300624114736721, 0.6066039755357417462, -231.5046416827383950 ) ) ;
#17722 = CARTESIAN_POINT ( 'NONE',  ( 27.02029988085337919, -0.4174685747284823112, -230.1188858631967378 ) ) ;
#17723 = CARTESIAN_POINT ( 'NONE',  ( -13.52935284690462758, -5.503084506376929141, -222.3607690796775671 ) ) ;
#17724 = CARTESIAN_POINT ( 'NONE',  ( -3.734153817218577309, -19.72686645808614614, -233.9207428641194610 ) ) ;
#17725 = CARTESIAN_POINT ( 'NONE',  ( -9.175187729848801155, 26.50888816229029743, -227.9285554593684253 ) ) ;
#17726 = CARTESIAN_POINT ( 'NONE',  ( 27.49181041625929467, 0.000000000000000000, 89.13175911166534604 ) ) ;
#17727 = CARTESIAN_POINT ( 'NONE',  ( -14.37318171526297483, 2.227741863946853140, -231.7654527934561202 ) ) ;
#17728 = CARTESIAN_POINT ( 'NONE',  ( -2.934221234790329369, 15.07857928364152222, -230.9558365497803720 ) ) ;
#17729 = CARTESIAN_POINT ( 'NONE',  ( -2.693916085894628942, 18.86613858709357672, -230.4911878356387263 ) ) ;
#17730 = ORIENTED_EDGE ( 'NONE', *, *, #1150, .T. ) ;
#17731 = AXIS2_PLACEMENT_3D ( 'NONE', #5180, #10153, #19026 ) ;
#17732 = ORIENTED_EDGE ( 'NONE', *, *, #2798, .F. ) ;
#17733 = AXIS2_PLACEMENT_3D ( 'NONE', #3123, #2891, #1851 ) ;
#17734 = CARTESIAN_POINT ( 'NONE',  ( -0.1881941282075867139, 17.37563936270229092, -230.9177995227891813 ) ) ;
#17735 = CARTESIAN_POINT ( 'NONE',  ( -27.32939371162572684, 5.861081283609568260, -224.9659309793921409 ) ) ;
#17736 = CARTESIAN_POINT ( 'NONE',  ( 10.90540179105271967, 5.382827416078996841, -224.1493061458977820 ) ) ;
#17737 = CARTESIAN_POINT ( 'NONE',  ( 8.767697218519710844, -14.65932909790238448, -230.8495237012982386 ) ) ;
#17738 = DIRECTION ( 'NONE',  ( 1.224646799147353207E-16, 1.000000000000000000, -0.000000000000000000 ) ) ;
#17739 = ORIENTED_EDGE ( 'NONE', *, *, #4471, .F. ) ;
#17740 = CARTESIAN_POINT ( 'NONE',  ( 7.743212835174657194, 11.90778931056080481, -226.0491028376908105 ) ) ;
#17741 = CARTESIAN_POINT ( 'NONE',  ( 18.57039993684838564, -7.499893981036622748, -219.4816775992414080 ) ) ;
#17742 = CARTESIAN_POINT ( 'NONE',  ( -23.00000000000000000, 0.000000000000000000, -55.00000000000000000 ) ) ;
#17743 = CARTESIAN_POINT ( 'NONE',  ( 0.5120693878963755719, -30.63998626839889639, -227.9504769009175220 ) ) ;
#17744 = SHAPE_DEFINITION_REPRESENTATION ( #15362, #9901 ) ;
#17745 = CARTESIAN_POINT ( 'NONE',  ( -11.24282496690421596, 12.44430180464951086, -232.4405891940542404 ) ) ;
#17747 = CARTESIAN_POINT ( 'NONE',  ( -7.752954785937490989, 10.21341112307795385, -225.5135920495299615 ) ) ;
#17746 = CIRCLE ( 'NONE', #11632, 3.000000000000002665 ) ;
#17748 = ORIENTED_EDGE ( 'NONE', *, *, #20398, .F. ) ;
#17749 = CARTESIAN_POINT ( 'NONE',  ( -6.282398543089500187, 12.01615879894893801, -228.5121145169883903 ) ) ;
#17750 = CARTESIAN_POINT ( 'NONE',  ( -10.22552941266963877, -9.699191453761107695, -225.4315674810442545 ) ) ;
#17751 = AXIS2_PLACEMENT_3D ( 'NONE', #197, #3560, #15617 ) ;
#17752 = DIRECTION ( 'NONE',  ( -1.000000000000000000, 0.000000000000000000, 0.000000000000000000 ) ) ;
#17753 = DIRECTION ( 'NONE',  ( -0.000000000000000000, -0.000000000000000000, 1.000000000000000000 ) ) ;
#17754 = CARTESIAN_POINT ( 'NONE',  ( -6.101488798441174310, 11.33371047077072369, -225.3616985956418546 ) ) ;
#17755 = CARTESIAN_POINT ( 'NONE',  ( 4.072690587420734865, -13.44063513242216246, -222.4530508649998239 ) ) ;
#17756 = CARTESIAN_POINT ( 'NONE',  ( 0.000000000000000000, 0.000000000000000000, -75.00000000000000000 ) ) ;
#17757 = CARTESIAN_POINT ( 'NONE',  ( -11.79584727357715934, 6.509288465425584036, -222.6080315736180921 ) ) ;
#17758 = CARTESIAN_POINT ( 'NONE',  ( 13.38540196930496862, 9.639609424068478205, -227.8779021328794840 ) ) ;
#17759 = CARTESIAN_POINT ( 'NONE',  ( -13.17897211815351000, 23.48099580033777301, -217.3415693533541173 ) ) ;
#17760 = DIRECTION ( 'NONE',  ( -1.000000000000000000, 0.000000000000000000, 0.000000000000000000 ) ) ;
#17761 = CARTESIAN_POINT ( 'NONE',  ( 16.53859560591101641, 22.24348416270211359, -223.7250258089275974 ) ) ;
#17762 = CARTESIAN_POINT ( 'NONE',  ( -8.370291489323296474, -27.15533861588617981, -226.3382906634514597 ) ) ;
#17763 = EDGE_LOOP ( 'NONE', ( #5484, #18862, #5152, #14529, #3376, #19412 ) ) ;
#17764 = CARTESIAN_POINT ( 'NONE',  ( -4.073886805163430935, 14.35067061637828623, -226.4733297826468572 ) ) ;
#17765 = CARTESIAN_POINT ( 'NONE',  ( -22.03660207690921879, 17.07234836129451949, -222.7335359861421296 ) ) ;
#17766 = CARTESIAN_POINT ( 'NONE',  ( -16.90193019167508126, 18.45790510038867893, -217.5707532411249758 ) ) ;
#17767 = CARTESIAN_POINT ( 'NONE',  ( -19.03657574603155567, -20.25511037490812782, -224.1171725289517269 ) ) ;
#17768 = CARTESIAN_POINT ( 'NONE',  ( 0.000000000000000000, 0.000000000000000000, -78.50000000000000000 ) ) ;
#17769 = ORIENTED_EDGE ( 'NONE', *, *, #8473, .F. ) ;
#17770 = CARTESIAN_POINT ( 'NONE',  ( -21.89482327431018760, 1.733733432562314158, -233.1353281693111796 ) ) ;
#17771 = CARTESIAN_POINT ( 'NONE',  ( 2.245945009347994237, -28.59251958642781233, -226.9771193766267743 ) ) ;
#17772 = CARTESIAN_POINT ( 'NONE',  ( 15.42212722119060864, 5.401662248084913465, -220.8333402320903645 ) ) ;
#17773 = VECTOR ( 'NONE', #19745, 1000.000000000000000 ) ;
#17774 = CARTESIAN_POINT ( 'NONE',  ( -5.807479211365208727, 19.77444019604324410, -216.0778658752277863 ) ) ;
#17775 = UNCERTAINTY_MEASURE_WITH_UNIT (LENGTH_MEASURE( 1.000000000000000082E-05 ), #3556, 'distance_accuracy_value', 'NONE');
#17776 = CARTESIAN_POINT ( 'NONE',  ( -17.91550223652134122, 4.809113705933536487, -230.6324822114035555 ) ) ;
#17777 = CARTESIAN_POINT ( 'NONE',  ( 23.04342321161690776, 14.90264581583150694, -218.4777833225197412 ) ) ;
#17778 = CARTESIAN_POINT ( 'NONE',  ( 15.85665641241444668, 18.24713744004561988, -217.7195292979064902 ) ) ;
#17779 = CARTESIAN_POINT ( 'NONE',  ( -10.76635261883074435, 0.3188271712753679710, 92.00000000000002842 ) ) ;
#17780 = CARTESIAN_POINT ( 'NONE',  ( -15.48425879135615446, -25.29886615046042309, -220.6886037686364261 ) ) ;
#17781 = CARTESIAN_POINT ( 'NONE',  ( 15.60497028854143764, -26.39208911975253002, -225.8550158017044112 ) ) ;
#17782 = CYLINDRICAL_SURFACE ( 'NONE', #14227, 25.00000000000000000 ) ;
#17783 = PRESENTATION_LAYER_ASSIGNMENT (  '', '', ( #19924 ) ) ;
#17784 = DIRECTION ( 'NONE',  ( 0.000000000000000000, 0.000000000000000000, -1.000000000000000000 ) ) ;
#17785 = CARTESIAN_POINT ( 'NONE',  ( -12.22073052649759184, 14.03927388329973525, -215.9097966823721606 ) ) ;
#17786 = CARTESIAN_POINT ( 'NONE',  ( -23.46219451118877330, -13.03948552059806509, -221.3852197888554372 ) ) ;
#17787 = CARTESIAN_POINT ( 'NONE',  ( -13.97943781666340790, 5.798109546139844639, -228.2992319913466019 ) ) ;
#17788 = CARTESIAN_POINT ( 'NONE',  ( 23.44028133050380802, 19.87677100428751231, -223.1503774981096342 ) ) ;
#17789 = CARTESIAN_POINT ( 'NONE',  ( -1.696080206444520844, 14.74162257415073540, -222.2455536759108838 ) ) ;
#17790 = ORIENTED_EDGE ( 'NONE', *, *, #19718, .T. ) ;
#17791 = CARTESIAN_POINT ( 'NONE',  ( 20.52151979663716830, -23.02670487196117222, -229.5295066797569348 ) ) ;
#17792 = CARTESIAN_POINT ( 'NONE',  ( 22.18132842682159733, 5.591149267797686839, -232.0584733989884114 ) ) ;
#17793 = CARTESIAN_POINT ( 'NONE',  ( 2.660414182604129429, 28.99288898680367055, -232.5781547115647072 ) ) ;
#17794 = CARTESIAN_POINT ( 'NONE',  ( -12.15711705271618470, 28.08001788883979799, -220.3431297925021681 ) ) ;
#17795 = CARTESIAN_POINT ( 'NONE',  ( -27.10757994293576800, -10.52107906247675473, -229.7403242048749519 ) ) ;
#17796 = CARTESIAN_POINT ( 'NONE',  ( -21.93900267957129557, 7.862893636934532360, -233.4951761057262161 ) ) ;
#17797 = DIRECTION ( 'NONE',  ( 0.000000000000000000, 0.000000000000000000, -1.000000000000000000 ) ) ;
#17798 = EDGE_CURVE ( 'NONE', #14639, #19932, #12570, .T. ) ;
#17799 = CARTESIAN_POINT ( 'NONE',  ( 14.56914850832129815, -2.041740472307377985, -224.7121590863160350 ) ) ;
#17800 = CARTESIAN_POINT ( 'NONE',  ( -2.047892494109819328, 12.88402507277750786, -223.5104301352110951 ) ) ;
#17801 = CARTESIAN_POINT ( 'NONE',  ( 13.21888801141564151, 2.135177519634172238, -228.0426311217386797 ) ) ;
#17802 = CARTESIAN_POINT ( 'NONE',  ( 15.92396645628901020, -0.3225394686005420009, -223.0199929375764327 ) ) ;
#17803 = CARTESIAN_POINT ( 'NONE',  ( 8.812073984913094904, 13.12649198322903210, -229.9172071780580495 ) ) ;
#17804 = CARTESIAN_POINT ( 'NONE',  ( -19.98462433625633494, -12.30084073857678639, -216.8518508258974862 ) ) ;
#17805 = EDGE_CURVE ( 'NONE', #2355, #12271, #5468, .T. ) ;
#17806 = EDGE_LOOP ( 'NONE', ( #1758, #3931, #8289, #9219 ) ) ;
#17807 = CARTESIAN_POINT ( 'NONE',  ( -1.707778556226592581, 19.51307486516442680, -232.5708079709245055 ) ) ;
#17808 = CARTESIAN_POINT ( 'NONE',  ( -1.489322793389167288, -21.37773154815333498, -215.8826219457350817 ) ) ;
#17809 = CARTESIAN_POINT ( 'NONE',  ( 5.169766346882679997, 29.28517558595074988, -221.5178724947562614 ) ) ;
#17810 = CARTESIAN_POINT ( 'NONE',  ( 8.134488596945347538, -11.59059696487595481, -231.6292735970982335 ) ) ;
#17811 = CARTESIAN_POINT ( 'NONE',  ( 1.526556658859590243E-13, -20.99999999999999645, 69.99999999999998579 ) ) ;
#17812 = CARTESIAN_POINT ( 'NONE',  ( -10.29720673141181209, 11.14783905173092649, -222.8560683878917530 ) ) ;
#17813 = SURFACE_STYLE_USAGE ( .BOTH. , #19264 ) ;
#17814 = CARTESIAN_POINT ( 'NONE',  ( -28.53682043726378836, -3.412203979905605866, -221.0207037827091767 ) ) ;
#17815 = CARTESIAN_POINT ( 'NONE',  ( 9.489894741926459432, 25.96007012349547338, -222.3210984495278524 ) ) ;
#17816 = CARTESIAN_POINT ( 'NONE',  ( -21.66803296057637951, 19.04503900041684616, -222.6603677762044526 ) ) ;
#17817 = CARTESIAN_POINT ( 'NONE',  ( 26.48990917286906921, 12.16675355942207659, -225.0153622588060216 ) ) ;
#17818 = CARTESIAN_POINT ( 'NONE',  ( -12.60888841760081824, -15.87650330583304914, -218.3826098682522456 ) ) ;
#17819 = AXIS2_PLACEMENT_3D ( 'NONE', #10800, #17559, #2236 ) ;
#17820 = COLOUR_RGB ( '', 0.08235294, 0.09019608, 0.10196078) ;
#17821 = CARTESIAN_POINT ( 'NONE',  ( 26.75877786246624623, 11.80320999550499117, -231.5572967531201414 ) ) ;
#17822 = DIRECTION ( 'NONE',  ( 0.000000000000000000, 0.000000000000000000, 1.000000000000000000 ) ) ;
#17823 = CARTESIAN_POINT ( 'NONE',  ( -7.876537541093066253, -10.96045937405908965, -230.9151686379251487 ) ) ;
#17824 = CARTESIAN_POINT ( 'NONE',  ( -1.038524475621362075, 14.89017051181998141, -222.3948816610352139 ) ) ;
#17825 = CARTESIAN_POINT ( 'NONE',  ( 16.96779410054824666, 23.69881408353223406, -220.2174342377987841 ) ) ;
#17826 = CARTESIAN_POINT ( 'NONE',  ( -8.900302563431933933, 20.17395648083808268, -216.9116515890487733 ) ) ;
#17827 = CARTESIAN_POINT ( 'NONE',  ( -4.155456637169709921, 11.30291311430030987, -225.2606024264729001 ) ) ;
#17828 = CARTESIAN_POINT ( 'NONE',  ( -21.89065952084848021, -0.9940043559354364566, -216.9999999999999716 ) ) ;
#17829 = ORIENTED_EDGE ( 'NONE', *, *, #7781, .F. ) ;
#17830 = CARTESIAN_POINT ( 'NONE',  ( 9.413533971304945069, -13.52850967935795623, -226.9656141048783695 ) ) ;
#17831 = CARTESIAN_POINT ( 'NONE',  ( 7.640685522499278903, -12.22373526560700441, -226.1755943870604710 ) ) ;
#17832 = DIRECTION ( 'NONE',  ( -0.000000000000000000, -0.000000000000000000, 1.000000000000000000 ) ) ;
#17833 = CARTESIAN_POINT ( 'NONE',  ( 18.46552355142154411, 5.019711608606525211, -231.5099115070375433 ) ) ;
#17834 = CARTESIAN_POINT ( 'NONE',  ( 19.06763123184207487, -2.048228142369658666, -218.2337357994572073 ) ) ;
#17835 = CARTESIAN_POINT ( 'NONE',  ( -14.13781561609191328, -15.90667165809925621, -233.6615929499251649 ) ) ;
#17836 = CARTESIAN_POINT ( 'NONE',  ( -1.489322793389167288, -21.37773154815333498, -215.8826219457350817 ) ) ;
#17837 = CARTESIAN_POINT ( 'NONE',  ( 3.528957931946373971, 27.43889307663531696, -223.4805233499528185 ) ) ;
#17838 = CARTESIAN_POINT ( 'NONE',  ( 0.000000000000000000, -17.50000000000000711, -60.00000000000000000 ) ) ;
#17839 = CARTESIAN_POINT ( 'NONE',  ( -12.13127060986278316, 5.971392262169284315, -229.0615017441034524 ) ) ;
#17840 = CARTESIAN_POINT ( 'NONE',  ( -3.368164009525018265, 19.03203264544105622, -233.5986411977714567 ) ) ;
#17841 = CARTESIAN_POINT ( 'NONE',  ( 3.060417506408009469, 27.46204888741655026, -226.6022202862033623 ) ) ;
#17842 = CARTESIAN_POINT ( 'NONE',  ( 22.70267758588118312, -6.899298642777032420, -215.6456595153534863 ) ) ;
#17843 = VERTEX_POINT ( 'NONE', #5914 ) ;
#17844 = ORIENTED_EDGE ( 'NONE', *, *, #19866, .T. ) ;
#17845 = CARTESIAN_POINT ( 'NONE',  ( 22.73582563804385970, 20.20868311426415431, -227.8513184012435886 ) ) ;
#17846 = CARTESIAN_POINT ( 'NONE',  ( -17.75632171729475317, 14.45153669854845901, -218.6240360064753929 ) ) ;
#17847 = CARTESIAN_POINT ( 'NONE',  ( 14.95834318372430083, -1.617016552789838801, -229.6306532055809271 ) ) ;
#17848 = CARTESIAN_POINT ( 'NONE',  ( -4.650330424930598561, -23.85841421069521928, -231.7493909980149454 ) ) ;
#17850 = DIRECTION ( 'NONE',  ( -0.000000000000000000, -0.000000000000000000, -1.000000000000000000 ) ) ;
#17849 = CIRCLE ( 'NONE', #18573, 4.100000000000000533 ) ;
#17851 = CARTESIAN_POINT ( 'NONE',  ( 0.000000000000000000, 0.000000000000000000, 75.00000000000000000 ) ) ;
#17852 = CARTESIAN_POINT ( 'NONE',  ( 15.91295838535984331, 21.88410254487826379, -230.9583961155862823 ) ) ;
#17853 = CARTESIAN_POINT ( 'NONE',  ( 26.20608998270887469, -2.199599969171641689, -229.6935040011478009 ) ) ;
#17854 = DIRECTION ( 'NONE',  ( -1.224646799147353207E-16, 1.000000000000000000, 0.000000000000000000 ) ) ;
#17855 = CARTESIAN_POINT ( 'NONE',  ( 6.427665535191954937, -16.40046818492683656, -232.5919299485929912 ) ) ;
#17856 = PRODUCT_CONTEXT ( 'NONE', #4828, 'mechanical' ) ;
#17857 = CARTESIAN_POINT ( 'NONE',  ( 2.008896548638861024, 20.64812324442097591, -233.5818019448501843 ) ) ;
#17858 = CARTESIAN_POINT ( 'NONE',  ( -24.30769394037691100, 17.48612956801762053, -223.4340414801748693 ) ) ;
#17859 = VERTEX_POINT ( 'NONE', #10875 ) ;
#17860 = CARTESIAN_POINT ( 'NONE',  ( -14.83974801774860630, 13.71714848582103485, -216.0935642439352762 ) ) ;
#17861 = CARTESIAN_POINT ( 'NONE',  ( -18.38002254392888446, -21.81807606669838506, -229.0374583293157968 ) ) ;
#17862 = FACE_OUTER_BOUND ( 'NONE', #11846, .T. ) ;
#17863 = DIRECTION ( 'NONE',  ( 0.000000000000000000, 0.000000000000000000, 1.000000000000000000 ) ) ;
#17864 = EDGE_CURVE ( 'NONE', #10566, #18119, #10193, .T. ) ;
#17865 = CARTESIAN_POINT ( 'NONE',  ( -11.26857159993117996, 28.96895336474501192, -225.6039696848669678 ) ) ;
#17866 = CARTESIAN_POINT ( 'NONE',  ( 2.697602325873029727, -29.85947730167685421, -229.1126320946688111 ) ) ;
#17867 = CARTESIAN_POINT ( 'NONE',  ( 14.93094482340519846, -1.857544602713102400, -222.6424950236294364 ) ) ;
#17868 = CARTESIAN_POINT ( 'NONE',  ( -23.49379658590067876, 11.46840048879614393, -217.2519070826072323 ) ) ;
#17869 = CARTESIAN_POINT ( 'NONE',  ( -12.88152464663890306, 6.317716727793897924, -230.5294309895745073 ) ) ;
#17870 = CARTESIAN_POINT ( 'NONE',  ( -1.268862717067444024, 15.25222216985846480, -229.0661283592426116 ) ) ;
#17871 = FACE_OUTER_BOUND ( 'NONE', #10685, .T. ) ;
#17872 = CARTESIAN_POINT ( 'NONE',  ( 20.62963957373278134, 2.372686805184054837, -232.5966151263358483 ) ) ;
#17873 = CARTESIAN_POINT ( 'NONE',  ( -19.03657574603155567, -20.25511037490812782, -224.1171725289517269 ) ) ;
#17874 = ORIENTED_EDGE ( 'NONE', *, *, #2321, .T. ) ;
#17875 = CARTESIAN_POINT ( 'NONE',  ( 6.491278574642851851, 13.23281603069746382, -229.0355254242266767 ) ) ;
#17876 = CARTESIAN_POINT ( 'NONE',  ( -12.01777041390050726, 10.97692933293401474, -227.6853890888168053 ) ) ;
#17877 = CARTESIAN_POINT ( 'NONE',  ( -14.01966324001334385, 10.60695606488527964, -217.6333332521996340 ) ) ;
#17878 = ORIENTED_EDGE ( 'NONE', *, *, #11148, .T. ) ;
#17879 = CARTESIAN_POINT ( 'NONE',  ( -22.16366393984728234, -4.852915104599624385, -232.2864540303542924 ) ) ;
#17880 = CARTESIAN_POINT ( 'NONE',  ( -22.56777165119825668, 3.065265347278306676E-15, 95.00000000000000000 ) ) ;
#17881 = ORIENTED_EDGE ( 'NONE', *, *, #12958, .F. ) ;
#17882 = CARTESIAN_POINT ( 'NONE',  ( -18.08305592660031991, 4.022743421239192152, -217.2335041149100050 ) ) ;
#17883 = CARTESIAN_POINT ( 'NONE',  ( 7.295492848317381984, -15.02116458630077034, -222.2946426130486941 ) ) ;
#17884 = CARTESIAN_POINT ( 'NONE',  ( 22.84140515590350518, 18.29101041979067332, -226.2334522600520472 ) ) ;
#17885 = CARTESIAN_POINT ( 'NONE',  ( 4.354034006296288339, 14.09944204372416188, -221.2519525881239417 ) ) ;
#17886 = CARTESIAN_POINT ( 'NONE',  ( -16.66921372850992000, 0.4301828684420727078, -227.8397539831347842 ) ) ;
#17887 = CARTESIAN_POINT ( 'NONE',  ( 20.02669998934234741, 11.93441252203826508, -216.7824909737982182 ) ) ;
#17888 = EDGE_CURVE ( 'NONE', #1956, #215, #7689, .T. ) ;
#17889 = CARTESIAN_POINT ( 'NONE',  ( 17.99029889091409018, 9.613712288440757092, -232.0298403238024036 ) ) ;
#17890 = DIRECTION ( 'NONE',  ( -0.000000000000000000, -0.000000000000000000, -1.000000000000000000 ) ) ;
#17891 = CARTESIAN_POINT ( 'NONE',  ( -15.27057301462635408, -17.00912219741827514, -233.6288396447818627 ) ) ;
#17892 = CARTESIAN_POINT ( 'NONE',  ( 5.668262076144046979, -25.28042871382391965, -216.8182873783340483 ) ) ;
#17893 = CARTESIAN_POINT ( 'NONE',  ( 0.000000000000000000, 0.000000000000000000, -77.51594804401857175 ) ) ;
#17894 = PLANE ( 'NONE',  #8011 ) ;
#17895 = CARTESIAN_POINT ( 'NONE',  ( -7.626320092023432196, 21.25423560278784407, -233.8867968595558295 ) ) ;
#17896 = CARTESIAN_POINT ( 'NONE',  ( 11.91821674756695693, -1.593691010653677242, -227.2895864140137405 ) ) ;
#17897 = CARTESIAN_POINT ( 'NONE',  ( 15.13105790938820228, -1.902449014147146178, -222.1588331224812407 ) ) ;
#17898 = CARTESIAN_POINT ( 'NONE',  ( 14.20064147608437821, 14.63411858269657806, -233.6150408276221242 ) ) ;
#17899 = CARTESIAN_POINT ( 'NONE',  ( 10.63406535173453271, 22.16595115341124256, -219.6461356279925781 ) ) ;
#17900 = VERTEX_POINT ( 'NONE', #12352 ) ;
#17901 = CARTESIAN_POINT ( 'NONE',  ( 26.97873870420736253, -17.71910932852193454, -225.8965020979516964 ) ) ;
#17902 = CARTESIAN_POINT ( 'NONE',  ( 14.49999999999999645, 2.015503622133300698, 92.99999999999998579 ) ) ;
#17903 = CARTESIAN_POINT ( 'NONE',  ( -5.373457274256926652, 30.83572167890261184, -229.2199105909169532 ) ) ;
#17904 = CARTESIAN_POINT ( 'NONE',  ( -5.568057711815838751, 28.69723585065299076, -232.1518503103610271 ) ) ;
#17905 = CARTESIAN_POINT ( 'NONE',  ( 21.75737151495774313, -2.205713500382427750, -233.2756072794337285 ) ) ;
#17906 = CARTESIAN_POINT ( 'NONE',  ( -24.02434186778878455, 18.57431834865475651, -228.2662945587547370 ) ) ;
#17907 = CARTESIAN_POINT ( 'NONE',  ( -21.50000000000001066, 0.000000000000000000, -65.00000000000000000 ) ) ;
#17908 = CARTESIAN_POINT ( 'NONE',  ( 22.14341918773124362, -7.622004812940091689, -217.4502831791021720 ) ) ;
#17909 = CARTESIAN_POINT ( 'NONE',  ( -6.593106361191484410, 26.27107262772703322, -231.8730401762632596 ) ) ;
#17910 = CARTESIAN_POINT ( 'NONE',  ( 16.22460398937575121, -0.7285105026664867589, -219.3274985887512116 ) ) ;
#17911 = CARTESIAN_POINT ( 'NONE',  ( -14.83974801774860630, 13.71714848582103485, -216.0935642439352762 ) ) ;
#17912 = CARTESIAN_POINT ( 'NONE',  ( 26.48990917286906921, 12.16675355942207659, -225.0153622588060216 ) ) ;
#17913 = CARTESIAN_POINT ( 'NONE',  ( 15.50884165284638705, 1.028647572718199843, -227.8181348745474679 ) ) ;
#17914 = EDGE_LOOP ( 'NONE', ( #5145, #11606, #399, #18671 ) ) ;
#17915 = CARTESIAN_POINT ( 'NONE',  ( 5.585286719045844173, 27.51657303716567426, -222.4190945945824751 ) ) ;
#17916 = CARTESIAN_POINT ( 'NONE',  ( -15.22366728182010043, -5.552021002219007961, -230.2511309519622671 ) ) ;
#17917 = CARTESIAN_POINT ( 'NONE',  ( 5.623554730548537606, 15.65270319720736225, -231.3185741195121068 ) ) ;
#17918 = CARTESIAN_POINT ( 'NONE',  ( -0.6614632862528592172, -26.57152937425246719, -233.3304277112415548 ) ) ;
#17919 = CARTESIAN_POINT ( 'NONE',  ( 20.29114891157137635, 1.643118446426296675, -222.4836142174464726 ) ) ;
#17920 = ADVANCED_FACE ( 'NONE', ( #19637 ), #10567, .F. ) ;
#17921 = CARTESIAN_POINT ( 'NONE',  ( -13.75208518020500748, 5.661250135068270239, -227.6647651141479685 ) ) ;
#17922 = CARTESIAN_POINT ( 'NONE',  ( 0.000000000000000000, -17.50000000000000711, -24.99999999999999645 ) ) ;
#17923 = CARTESIAN_POINT ( 'NONE',  ( 13.37423534347618670, -3.100899090186935325, -222.2483675785374260 ) ) ;
#17924 = CARTESIAN_POINT ( 'NONE',  ( 9.382249691333727881, 26.55946126407900820, -224.4468135941759215 ) ) ;
#17925 = CARTESIAN_POINT ( 'NONE',  ( -13.96147744945181124, 5.260363697127891314, -222.3342733685200301 ) ) ;
#17927 = AXIS2_PLACEMENT_3D ( 'NONE', #16510, #6717, #17180 ) ;
#17926 = CARTESIAN_POINT ( 'NONE',  ( -27.53108621362071773, 14.15137273650544536, -219.7961709676081625 ) ) ;
#17928 = CARTESIAN_POINT ( 'NONE',  ( -10.89162261547930655, -11.18732543557264592, -227.7569336215896953 ) ) ;
#17929 = CARTESIAN_POINT ( 'NONE',  ( 22.49659352743751128, 7.060662713609715979, -215.7089950799439180 ) ) ;
#17930 = CLOSED_SHELL ( 'NONE', ( #13412, #2192, #5939, #10797, #4169, #17310, #1311, #14862, #20693, #9600, #16889, #16669, #18065, #18766, #9300, #1686, #9735, #19033, #19818, #17108, #19225, #751, #13410, #5698, #6230 ) ) ;
#17931 = DIRECTION ( 'NONE',  ( -0.000000000000000000, -0.000000000000000000, -1.000000000000000000 ) ) ;
#17932 = CARTESIAN_POINT ( 'NONE',  ( -13.21307282338718991, -4.958223064515467016, -219.4340824732878730 ) ) ;
#17933 = CARTESIAN_POINT ( 'NONE',  ( -1.433739110790628102, 17.19322394474796667, -219.1420620387681879 ) ) ;
#17934 = CARTESIAN_POINT ( 'NONE',  ( -19.67797246974518544, 1.229961341702398681, -219.4743747885323160 ) ) ;
#17935 = CARTESIAN_POINT ( 'NONE',  ( -17.07311071032027172, 18.59516984069744794, -230.9440421721702137 ) ) ;
#17936 = CIRCLE ( 'NONE', #336, 23.00000000000008882 ) ;
#17937 = CARTESIAN_POINT ( 'NONE',  ( 4.952019330116582907, 28.88045068338265509, -217.6369327391592208 ) ) ;
#17938 = CARTESIAN_POINT ( 'NONE',  ( -3.077342110593487945, -14.65776296416898816, -220.8866639047373610 ) ) ;
#17939 = CARTESIAN_POINT ( 'NONE',  ( 1.525817648051120967, -14.82969601928396841, -225.8796824437346515 ) ) ;
#17940 = DIRECTION ( 'NONE',  ( -1.000000000000000000, 0.000000000000000000, 0.000000000000000000 ) ) ;
#17941 = CARTESIAN_POINT ( 'NONE',  ( 13.03557269046774714, 7.519834803053426775, -226.9490612297269081 ) ) ;
#17942 = CARTESIAN_POINT ( 'NONE',  ( 22.14671607713456325, -14.13547298543019437, -218.1897693226341914 ) ) ;
#17943 = CARTESIAN_POINT ( 'NONE',  ( -21.28605893225895684, -20.43870967537180050, -221.0356759888913700 ) ) ;
#17944 = CARTESIAN_POINT ( 'NONE',  ( -5.902479482706956659, -14.78727544128710214, -218.5565286504736946 ) ) ;
#17945 = CARTESIAN_POINT ( 'NONE',  ( 6.402706778685327116, 14.41397785959879307, -226.0127495172349086 ) ) ;
#17946 = DIRECTION ( 'NONE',  ( 4.408728476930466911E-15, -1.000000000000000000, 0.000000000000000000 ) ) ;
#17947 = CARTESIAN_POINT ( 'NONE',  ( 17.32394486779715592, 4.028159306070694612, -218.4253989884176690 ) ) ;
#17948 = CARTESIAN_POINT ( 'NONE',  ( 0.9046320824004248085, 13.39785254849979701, -226.4815711199935890 ) ) ;
#17949 = CARTESIAN_POINT ( 'NONE',  ( 0.9458336400950161371, 17.49535648476021876, -228.8359568483051589 ) ) ;
#17950 = CARTESIAN_POINT ( 'NONE',  ( 12.64197975508134597, -4.295353707277522304, -228.6481500018833799 ) ) ;
#17951 = ORIENTED_EDGE ( 'NONE', *, *, #19702, .F. ) ;
#17952 = CARTESIAN_POINT ( 'NONE',  ( 9.774133712851615030, 11.09751083462123766, -229.6876724410067823 ) ) ;
#17953 = CARTESIAN_POINT ( 'NONE',  ( -13.92941769543345032, 11.48925904027772127, -219.8938199480626281 ) ) ;
#17954 = CARTESIAN_POINT ( 'NONE',  ( 11.21112214669106777, 5.418350954422431975, -227.6539796508718325 ) ) ;
#17955 = CARTESIAN_POINT ( 'NONE',  ( -4.253447013113726527, -22.64852647464574531, -232.0531923962242615 ) ) ;
#17956 = CARTESIAN_POINT ( 'NONE',  ( 0.000000000000000000, 0.000000000000000000, -69.99999999999998579 ) ) ;
#17957 = ORIENTED_EDGE ( 'NONE', *, *, #19709, .F. ) ;
#17958 = CARTESIAN_POINT ( 'NONE',  ( 10.50530447320976535, 20.19629329636330084, -217.1354359361034767 ) ) ;
#17959 = CARTESIAN_POINT ( 'NONE',  ( 18.46162736253148395, -12.23454570505295358, -218.9425382959138062 ) ) ;
#17960 = CARTESIAN_POINT ( 'NONE',  ( -16.32047052250102581, 2.570795953410685009, -230.9329235942756213 ) ) ;
#17961 = EDGE_CURVE ( 'NONE', #11, #5879, #13437, .T. ) ;
#17962 = CARTESIAN_POINT ( 'NONE',  ( -8.878187501988019648, -11.23476449186280846, -221.0271673637577123 ) ) ;
#17963 = PRODUCT_CONTEXT ( 'NONE', #19060, 'mechanical' ) ;
#17964 = CARTESIAN_POINT ( 'NONE',  ( -0.1571923090946999446, 19.34188126963334398, -216.6893131123363787 ) ) ;
#17965 = CARTESIAN_POINT ( 'NONE',  ( -0.4465333940385243228, 12.27026616490476485, -221.3722328744566425 ) ) ;
#17966 = ORIENTED_EDGE ( 'NONE', *, *, #4601, .F. ) ;
#17967 = CARTESIAN_POINT ( 'NONE',  ( -18.09776816382430908, 23.50806826204562583, -229.9568677523880638 ) ) ;
#17968 = CARTESIAN_POINT ( 'NONE',  ( 25.79934686323926840, -4.908228874239597417, -218.4849570602390543 ) ) ;
#17969 = CARTESIAN_POINT ( 'NONE',  ( 0.000000000000000000, 21.00000000000000000, -75.00000000000000000 ) ) ;
#17970 = DIRECTION ( 'NONE',  ( 0.000000000000000000, 0.000000000000000000, 1.000000000000000000 ) ) ;
#17971 = CARTESIAN_POINT ( 'NONE',  ( -11.33137429837660193, 27.25022425932026238, -230.1650924901870212 ) ) ;
#17972 = CARTESIAN_POINT ( 'NONE',  ( 7.337960271553932046, -12.57654522398025065, -224.9099165242034530 ) ) ;
#17973 = CARTESIAN_POINT ( 'NONE',  ( 27.32546652195855685, -7.354568365469916991, -229.0866163655393279 ) ) ;
#17974 = CARTESIAN_POINT ( 'NONE',  ( -18.70100282803782576, 16.58357028540773115, -216.4425743468854080 ) ) ;
#17975 = CARTESIAN_POINT ( 'NONE',  ( -16.36835685385702988, 8.002698209344293545, -233.7585018083067894 ) ) ;
#17976 = ORIENTED_EDGE ( 'NONE', *, *, #16436, .F. ) ;
#17977 = CARTESIAN_POINT ( 'NONE',  ( -1.696080206444520844, 14.74162257415073540, -222.2455536759108838 ) ) ;
#17978 = DIRECTION ( 'NONE',  ( 1.000000000000000000, 0.000000000000000000, 0.000000000000000000 ) ) ;
#17979 = CARTESIAN_POINT ( 'NONE',  ( -20.05025075566126702, 1.207204931470905018, -215.1628017022767949 ) ) ;
#17980 = CARTESIAN_POINT ( 'NONE',  ( -13.60885102855131201, -21.92822159330905762, -220.4851091041354607 ) ) ;
#17981 = ORIENTED_EDGE ( 'NONE', *, *, #6515, .F. ) ;
#17982 = CARTESIAN_POINT ( 'NONE',  ( 13.82984244654956107, 22.51831320572884820, -232.1830460045772213 ) ) ;
#17983 = CARTESIAN_POINT ( 'NONE',  ( -6.094651895680649467, 13.59752566126439177, -221.0608041154719103 ) ) ;
#17984 = CARTESIAN_POINT ( 'NONE',  ( -14.98215928292561294, 22.79623052288931362, -230.3289734367122890 ) ) ;
#17985 = CARTESIAN_POINT ( 'NONE',  ( -15.02851318684991000, -5.270497739200964205, -221.5518599052197146 ) ) ;
#17986 = DIRECTION ( 'NONE',  ( -1.000000000000000000, 0.000000000000000000, 0.000000000000000000 ) ) ;
#17987 = VERTEX_POINT ( 'NONE', #5798 ) ;
#17988 = CARTESIAN_POINT ( 'NONE',  ( 19.30248206944178335, -1.297331563427565726, -230.8957665284791290 ) ) ;
#17989 = CARTESIAN_POINT ( 'NONE',  ( -5.100309671427054603, -23.83006135775530510, -217.1425084463234612 ) ) ;
#17990 = CARTESIAN_POINT ( 'NONE',  ( 14.23581535094758266, 1.730511134508401438, -227.4509761555696628 ) ) ;
#17991 = CARTESIAN_POINT ( 'NONE',  ( 4.484811161826725900, 15.38298568785217313, -219.4617573400562662 ) ) ;
#17992 = DIRECTION ( 'NONE',  ( -1.000000000000000000, 0.000000000000000000, 0.000000000000000000 ) ) ;
#17993 = CARTESIAN_POINT ( 'NONE',  ( -22.32700334442577272, 3.978587747811427988, -218.4803616146862453 ) ) ;
#17994 = CARTESIAN_POINT ( 'NONE',  ( 20.05374812456133782, 24.17492691056345677, -223.1494843338164458 ) ) ;
#17995 = CARTESIAN_POINT ( 'NONE',  ( 13.69275646168278371, 8.674223198772375909, -220.8699857572541987 ) ) ;
#17996 = DIRECTION ( 'NONE',  ( -0.1736481776669307198, 2.126576849575776229E-17, 0.9848077530122080203 ) ) ;
#17997 = CARTESIAN_POINT ( 'NONE',  ( -26.26363215285178043, -18.18116807333735352, -227.1727963224598739 ) ) ;
#17998 = CARTESIAN_POINT ( 'NONE',  ( -7.349743644505656093, -15.31718010764164539, -232.4470764718129772 ) ) ;
#17999 = CARTESIAN_POINT ( 'NONE',  ( 5.982950994121768673, -14.58086824529316594, -231.1438280359330975 ) ) ;
#18000 = CARTESIAN_POINT ( 'NONE',  ( 0.000000000000000000, 0.000000000000000000, 80.43141006107198621 ) ) ;
#18001 = DIRECTION ( 'NONE',  ( 1.000000000000000000, 0.000000000000000000, 0.000000000000000000 ) ) ;
#18002 = CARTESIAN_POINT ( 'NONE',  ( -1.837924626891132229, 29.27703531260187475, -227.2344808100871774 ) ) ;
#18003 = CARTESIAN_POINT ( 'NONE',  ( 26.96734317869073294, -1.796611605495658681, -216.2358245450472509 ) ) ;
#18004 = CARTESIAN_POINT ( 'NONE',  ( 28.22932473237819551, -8.039268142081398949, -226.6539694142420558 ) ) ;
#18005 = CARTESIAN_POINT ( 'NONE',  ( -17.49393085256189906, 10.63366922396483361, -217.7502683347138657 ) ) ;
#18006 = CARTESIAN_POINT ( 'NONE',  ( 16.96779410054824666, 23.69881408353223406, -220.2174342377987841 ) ) ;
#18007 = CARTESIAN_POINT ( 'NONE',  ( 10.12648780932046755, 24.76571117977573522, -228.8499436907259792 ) ) ;
#18008 = ORIENTED_EDGE ( 'NONE', *, *, #440, .F. ) ;
#18009 = CARTESIAN_POINT ( 'NONE',  ( 4.375292991814291987, -28.67199747747994465, -220.8092881619367631 ) ) ;
#18010 = FACE_OUTER_BOUND ( 'NONE', #11425, .T. ) ;
#18011 = CARTESIAN_POINT ( 'NONE',  ( -0.2758005215353623862, 11.79991891162212525, -226.8645588387054488 ) ) ;
#18012 = CARTESIAN_POINT ( 'NONE',  ( -4.334570222994868161, 11.62786715207288601, -222.6396919303362267 ) ) ;
#18013 = CARTESIAN_POINT ( 'NONE',  ( 18.84909589690502685, -4.856542942594316514, -217.9726137486037771 ) ) ;
#18014 = CARTESIAN_POINT ( 'NONE',  ( -8.501641725227710111, 25.47064987787527102, -217.3358698761548737 ) ) ;
#18015 = CARTESIAN_POINT ( 'NONE',  ( -23.03038449397558196, 2.820408665368003469E-15, 75.34729635533385306 ) ) ;
#18016 = CARTESIAN_POINT ( 'NONE',  ( -5.974114889119001681, 17.52937113675171332, -232.3862906442651592 ) ) ;
#18017 = CARTESIAN_POINT ( 'NONE',  ( 25.30941179858102430, 8.661697827793627624, -216.7530520919057722 ) ) ;
#18018 = CARTESIAN_POINT ( 'NONE',  ( -17.88126539071149779, 5.766250685202066961, -232.9050303536861293 ) ) ;
#18019 = CARTESIAN_POINT ( 'NONE',  ( 16.38151749656409351, 8.902090001712490874, -231.2955017965201989 ) ) ;
#18020 = CARTESIAN_POINT ( 'NONE',  ( -29.74115761720981510, -1.844952462305729401, -220.6656484738778943 ) ) ;
#18021 = ORIENTED_EDGE ( 'NONE', *, *, #12996, .F. ) ;
#18022 = CARTESIAN_POINT ( 'NONE',  ( -3.130305314451475418, 18.08417128930788209, -217.9058652980469333 ) ) ;
#18023 = CARTESIAN_POINT ( 'NONE',  ( -13.33530847390368024, -5.065163879519744228, -226.5386329521395226 ) ) ;
#18024 = CARTESIAN_POINT ( 'NONE',  ( 11.62313423782632782, 11.98467543564608029, -219.7293303032897995 ) ) ;
#18025 = CARTESIAN_POINT ( 'NONE',  ( -7.928105003701093167, -26.09134507487772225, -231.8683635223868578 ) ) ;
#18026 = DIRECTION ( 'NONE',  ( 4.408728476930466911E-15, -1.000000000000000000, 0.000000000000000000 ) ) ;
#18027 = CARTESIAN_POINT ( 'NONE',  ( -26.19327040236159831, 13.44417515682194875, -223.7810975255189874 ) ) ;
#18028 = CARTESIAN_POINT ( 'NONE',  ( 0.000000000000000000, 0.000000000000000000, 0.000000000000000000 ) ) ;
#18029 = CARTESIAN_POINT ( 'NONE',  ( 9.338484253624125486, -13.53666216847648052, -219.8958652322373837 ) ) ;
#18030 = CARTESIAN_POINT ( 'NONE',  ( 3.635089269978064141, 27.05650967970794341, -222.4639105745756638 ) ) ;
#18031 = CARTESIAN_POINT ( 'NONE',  ( -16.07193224038526580, 12.24477688577882439, -232.1409653212175499 ) ) ;
#18032 = CARTESIAN_POINT ( 'NONE',  ( -16.85225081326727903, 6.237400186851330020, -234.5847093771173206 ) ) ;
#18033 = CARTESIAN_POINT ( 'NONE',  ( -13.98007945013786291, -9.257046693524761949, -228.3752161438062842 ) ) ;
#18034 = CARTESIAN_POINT ( 'NONE',  ( 19.13589083395335422, 16.69125564174534659, -234.7442498487877174 ) ) ;
#18035 = AXIS2_PLACEMENT_3D ( 'NONE', #2741, #13323, #6344 ) ;
#18036 = CARTESIAN_POINT ( 'NONE',  ( 4.814824860968089633E-30, 19.63401512838754215, -77.51594804401857175 ) ) ;
#18037 = CARTESIAN_POINT ( 'NONE',  ( -17.24073315697368969, -20.31883122441189826, -234.2947248507418863 ) ) ;
#18038 = CARTESIAN_POINT ( 'NONE',  ( 5.359747511823000465, 20.14556701535824601, -232.9094821222151381 ) ) ;
#18039 = CARTESIAN_POINT ( 'NONE',  ( 13.86383614057800884, 4.939477956453596441, -219.6543243356308324 ) ) ;
#18040 = ADVANCED_FACE ( 'NONE', ( #16169 ), #739, .T. ) ;
#18041 = CARTESIAN_POINT ( 'NONE',  ( -5.727886109716582297, 15.25217619989539486, -230.5419623196804650 ) ) ;
#18042 = CARTESIAN_POINT ( 'NONE',  ( 12.03015173539790617, 23.46358517874481109, -216.0611092640310744 ) ) ;
#18043 = CARTESIAN_POINT ( 'NONE',  ( -5.100309671427054603, -23.83006135775530510, -217.1425084463234612 ) ) ;
#18044 = CARTESIAN_POINT ( 'NONE',  ( 1.250172743705837641, -19.35180105203422940, -231.6553945523530729 ) ) ;
#18045 = AXIS2_PLACEMENT_3D ( 'NONE', #2472, #16324, #7778 ) ;
#18046 = CARTESIAN_POINT ( 'NONE',  ( 14.98418162551161714, 4.450317369940187895, -227.9894155827521161 ) ) ;
#18047 = CARTESIAN_POINT ( 'NONE',  ( 18.22947608839760747, -6.525328669204546905, -217.7409786913911205 ) ) ;
#18048 = CARTESIAN_POINT ( 'NONE',  ( 13.78060503451313323, -0.3076571220309521904, -222.4352540772387101 ) ) ;
#18049 = CARTESIAN_POINT ( 'NONE',  ( -13.05629324012484282, -10.24599397043673221, -218.7452066004821347 ) ) ;
#18050 = CARTESIAN_POINT ( 'NONE',  ( 2.445562843591592372, 25.89340784564244657, -229.2671352353737859 ) ) ;
#18051 = CARTESIAN_POINT ( 'NONE',  ( 20.62963957373278134, 2.372686805184054837, -232.5966151263358483 ) ) ;
#18052 = CARTESIAN_POINT ( 'NONE',  ( 5.331555957413248059, 27.50712867803999728, -219.0801070358024276 ) ) ;
#18053 = CARTESIAN_POINT ( 'NONE',  ( 3.755404788550845474, 24.96758616565139022, -220.0839658302907935 ) ) ;
#18054 = CARTESIAN_POINT ( 'NONE',  ( 19.91550388961935525, -0.5333217442993671842, -216.6463151812154138 ) ) ;
#18055 = VERTEX_POINT ( 'NONE', #3783 ) ;
#18056 = CARTESIAN_POINT ( 'NONE',  ( 13.48097272627202159, 8.509510470709432894, -231.5257201610278059 ) ) ;
#18057 = CARTESIAN_POINT ( 'NONE',  ( -21.26441444091935296, 10.69428164102106926, -219.3434466924981336 ) ) ;
#18058 = CARTESIAN_POINT ( 'NONE',  ( -28.05279008194460744, 4.018900919424986284, -224.6698354068587662 ) ) ;
#18059 = CARTESIAN_POINT ( 'NONE',  ( -0.3025942668150596315, -28.96010673020088788, -223.5534481764385646 ) ) ;
#18060 = CARTESIAN_POINT ( 'NONE',  ( 1.665334536937735316E-13, -24.63401512838760610, -77.51594804401857175 ) ) ;
#18061 = FACE_OUTER_BOUND ( 'NONE', #10806, .T. ) ;
#18062 = CARTESIAN_POINT ( 'NONE',  ( 23.04897566969193079, 17.95862962700741861, -223.6438515760422661 ) ) ;
#18063 = CARTESIAN_POINT ( 'NONE',  ( 21.15565078817875388, -13.66792796406074295, -219.8984673185389624 ) ) ;
#18064 = CARTESIAN_POINT ( 'NONE',  ( -2.775557561562891351E-14, 0.000000000000000000, -105.0000000000000142 ) ) ;
#18065 = ADVANCED_FACE ( 'NONE', ( #10993, #17862 ), #14046, .T. ) ;
#18066 = CARTESIAN_POINT ( 'NONE',  ( -6.870552667427666904, -18.85419487977974029, -216.2130481585807047 ) ) ;
#18067 = APPLICATION_PROTOCOL_DEFINITION ( 'draft international standard', 'automotive_design', 1998, #9447 ) ;
#18068 = CARTESIAN_POINT ( 'NONE',  ( 4.559463107227270662, 13.27337529356814017, -226.9596205199204633 ) ) ;
#18069 = CARTESIAN_POINT ( 'NONE',  ( 2.660414182604129429, 28.99288898680367055, -232.5781547115647072 ) ) ;
#18070 = ORIENTED_EDGE ( 'NONE', *, *, #4766, .F. ) ;
#18071 = CARTESIAN_POINT ( 'NONE',  ( -6.201839134465864767, 11.37481922992157379, -223.7040893475979146 ) ) ;
#18072 = CARTESIAN_POINT ( 'NONE',  ( -29.05925532287432489, -3.238226816112620199, -230.1495230746535867 ) ) ;
#18073 = CARTESIAN_POINT ( 'NONE',  ( 27.54201077264015396, -3.286392687948289648, -218.1575117614944190 ) ) ;
#18074 = CARTESIAN_POINT ( 'NONE',  ( -20.86829502391188029, 9.671354583073858535, 2.626725457081121373 ) ) ;
#18075 = CARTESIAN_POINT ( 'NONE',  ( -8.823862513872974489, 14.92351368520778898, -217.1499513473673346 ) ) ;
#18076 = CARTESIAN_POINT ( 'NONE',  ( -21.92622494339052608, -22.07770017127804962, -220.0303431275545165 ) ) ;
#18077 = VECTOR ( 'NONE', #5870, 999.9999999999998863 ) ;
#18078 = CARTESIAN_POINT ( 'NONE',  ( 26.54225689383817866, -6.924125931238839016, -230.1506921200174247 ) ) ;
#18079 = CARTESIAN_POINT ( 'NONE',  ( -14.73016414256368911, 22.23431809695627237, -217.1425123644553707 ) ) ;
#18080 = CIRCLE ( 'NONE', #17009, 19.79999999999999716 ) ;
#18081 = CARTESIAN_POINT ( 'NONE',  ( -15.64716994811699813, 6.210654946517923491, -217.0002936794128345 ) ) ;
#18082 = EDGE_CURVE ( 'NONE', #2515, #14027, #10665, .T. ) ;
#18083 = CARTESIAN_POINT ( 'NONE',  ( 3.522445101072706475, 23.08420003150784439, -231.7850044194335055 ) ) ;
#18084 = DIRECTION ( 'NONE',  ( -0.000000000000000000, 0.000000000000000000, -1.000000000000000000 ) ) ;
#18085 = CARTESIAN_POINT ( 'NONE',  ( -12.10179538005628963, 1.685214252672075030, -222.4835512146784424 ) ) ;
#18086 = CARTESIAN_POINT ( 'NONE',  ( -17.56620462375804692, -17.71942105192161065, -219.9081625180047013 ) ) ;
#18087 = EDGE_LOOP ( 'NONE', ( #2981, #1041 ) ) ;
#18088 = CARTESIAN_POINT ( 'NONE',  ( 16.96779410054824666, 23.69881408353223406, -220.2174342377987841 ) ) ;
#18089 = CARTESIAN_POINT ( 'NONE',  ( 1.660345614755502686, 12.19060476922103931, -223.1112690039082906 ) ) ;
#18090 = CARTESIAN_POINT ( 'NONE',  ( -19.94037810645588138, 20.40093185429846656, -220.0593903119159620 ) ) ;
#18091 = CARTESIAN_POINT ( 'NONE',  ( -15.57180599510074437, -4.609960555941468918, -228.7341395176208323 ) ) ;
#18092 = EDGE_CURVE ( 'NONE', #9851, #12391, #15480, .T. ) ;
#18093 = CARTESIAN_POINT ( 'NONE',  ( 26.00000000000000000, 0.5000000000000000000, -6.000000000000000000 ) ) ;
#18094 = ORIENTED_EDGE ( 'NONE', *, *, #2125, .T. ) ;
#18095 = CARTESIAN_POINT ( 'NONE',  ( -18.46722752239034193, 0.9784074152395518809, -232.1633353206286188 ) ) ;
#18096 = CARTESIAN_POINT ( 'NONE',  ( -13.04380155829002419, -28.08004287256819609, -224.7912146079995352 ) ) ;
#18097 = CARTESIAN_POINT ( 'NONE',  ( 24.58316096239279602, 5.861425670879941485, -231.3104446318280623 ) ) ;
#18098 = CARTESIAN_POINT ( 'NONE',  ( -3.060450601941519189, 13.29454208326677289, -222.0135664617158682 ) ) ;
#18099 = DIRECTION ( 'NONE',  ( 0.000000000000000000, 0.000000000000000000, -1.000000000000000000 ) ) ;
#18100 = VECTOR ( 'NONE', #8476, 1000.000000000000000 ) ;
#18101 = AXIS2_PLACEMENT_3D ( 'NONE', #8537, #13599, #8757 ) ;
#18102 = CARTESIAN_POINT ( 'NONE',  ( -24.49083850720273148, 4.222094140707651100, -219.1543001448025905 ) ) ;
#18103 = CARTESIAN_POINT ( 'NONE',  ( 10.82528077991200810, 8.849546035972329250, -221.2068619981234008 ) ) ;
#18104 = CARTESIAN_POINT ( 'NONE',  ( -24.24581955882289819, 6.099808590248922080, -7.930829530152172069 ) ) ;
#18105 = CARTESIAN_POINT ( 'NONE',  ( 20.23125423326388628, 7.836699765464857137, -217.8891354894872450 ) ) ;
#18106 = DIRECTION ( 'NONE',  ( -1.000000000000000000, 0.000000000000000000, 0.000000000000000000 ) ) ;
#18107 = CARTESIAN_POINT ( 'NONE',  ( 20.39962514764921409, -3.647888038500222141, -219.1338420190236036 ) ) ;
#18108 = CARTESIAN_POINT ( 'NONE',  ( -15.15819830826754355, -2.370657588173597841, -221.8013720140894236 ) ) ;
#18109 = DIRECTION ( 'NONE',  ( -0.000000000000000000, -0.000000000000000000, -1.000000000000000000 ) ) ;
#18110 = CARTESIAN_POINT ( 'NONE',  ( -21.99162546567091425, 0.000000000000000000, -78.50000000000000000 ) ) ;
#18111 = B_SPLINE_CURVE_WITH_KNOTS ( 'NONE', 3,
 ( #4269, #2693, #7554, #19460, #14316, #7887, #16107, #4372, #19789, #21255, #21478, #12615, #5736, #680, #14749, #21590, #5847, #19903, #4049, #9464, #7448, #9247, #11147, #9575, #14422, #6179, #12944, #1012, #11041, #4160 ),
 .UNSPECIFIED., .F., .F.,
 ( 4, 1, 1, 1, 1, 1, 2, 2, 1, 1, 1, 1, 1, 2, 2, 1, 1, 1, 1, 2, 2, 4 ),
 ( 0.5000000000000000000, 0.5624999999999992228, 0.5937499999999988898, 0.6093749999999986677, 0.6171874999999985567, 0.6210937499999984457, 0.6230468749999984457, 0.6249999999999984457, 0.6874999999999985567, 0.7187499999999985567, 0.7343749999999986677, 0.7421874999999986677, 0.7460937499999986677, 0.7480468749999986677, 0.7499999999999986677, 0.8124999999999988898, 0.8437499999999988898, 0.8593749999999988898, 0.8671874999999988898, 0.8710937499999988898, 0.8749999999999988898, 1.000000000000000000 ),
 .UNSPECIFIED. ) ;
#18112 = CARTESIAN_POINT ( 'NONE',  ( -16.13584396029534318, 23.78382729893626646, -231.6788043429177435 ) ) ;
#18113 = CARTESIAN_POINT ( 'NONE',  ( 10.41909793732091494, -5.130961835214151279, -225.2553394319931783 ) ) ;
#18114 = CIRCLE ( 'NONE', #15969, 1.000000000000013323 ) ;
#18115 = CARTESIAN_POINT ( 'NONE',  ( 26.48152825632016061, -2.044474411990439666, -219.3412966555575565 ) ) ;
#18116 = CARTESIAN_POINT ( 'NONE',  ( -13.31590776630363315, 5.340120742929252096, -225.6956515496373186 ) ) ;
#18117 = CARTESIAN_POINT ( 'NONE',  ( 17.97920459523930958, 17.43922474653955490, -233.2737719749805763 ) ) ;
#18118 = CARTESIAN_POINT ( 'NONE',  ( 7.497537106193371770, 19.52448593130572618, -231.1338690134634248 ) ) ;
#18119 = VERTEX_POINT ( 'NONE', #13003 ) ;
#18120 = CARTESIAN_POINT ( 'NONE',  ( 6.644147376113458847, -12.60537238651543923, -230.3381876225809037 ) ) ;
#18121 = CARTESIAN_POINT ( 'NONE',  ( 0.000000000000000000, 0.000000000000000000, 94.00000000000000000 ) ) ;
#18122 = CARTESIAN_POINT ( 'NONE',  ( -5.467362224022371819, 23.92882567691090046, -234.7811165710531611 ) ) ;
#18123 = CARTESIAN_POINT ( 'NONE',  ( -15.46752262371512820, 15.15798787883389487, -233.5981584775992701 ) ) ;
#18124 = CARTESIAN_POINT ( 'NONE',  ( 17.03334375980016446, -6.184066897328505341, -231.2622903164569834 ) ) ;
#18125 = CARTESIAN_POINT ( 'NONE',  ( -1.249406995060579062, 25.48934319316224162, -216.9406480707515072 ) ) ;
#18126 = DIRECTION ( 'NONE',  ( -0.1736481776669307198, 2.126576849575776229E-17, 0.9848077530122080203 ) ) ;
#18127 = CARTESIAN_POINT ( 'NONE',  ( 2.987882271643250931, 28.57355997650491020, -217.8917278841813925 ) ) ;
#18128 = CARTESIAN_POINT ( 'NONE',  ( 15.87399429023076003, -1.683916961781461552, -230.8621029165058758 ) ) ;
#18129 = CARTESIAN_POINT ( 'NONE',  ( -17.39699619235753048, 15.64332637722790054, -216.0406373264262641 ) ) ;
#18130 = AXIS2_PLACEMENT_3D ( 'NONE', #16065, #7728, #21319 ) ;
#18131 = CARTESIAN_POINT ( 'NONE',  ( 22.18132842682159733, 5.591149267797686839, -232.0584733989884114 ) ) ;
#18132 = CARTESIAN_POINT ( 'NONE',  ( 9.214796078729456497, 26.59493510027307650, -225.5796848805584318 ) ) ;
#18133 = DIRECTION ( 'NONE',  ( 1.000000000000000000, 0.000000000000000000, 0.000000000000000000 ) ) ;
#18134 = ORIENTED_EDGE ( 'NONE', *, *, #7546, .T. ) ;
#18135 = CARTESIAN_POINT ( 'NONE',  ( 10.90137817157632227, 16.64712710991609868, -230.5401786220292593 ) ) ;
#18136 = CARTESIAN_POINT ( 'NONE',  ( -15.27057301462635408, -17.00912219741827514, -233.6288396447818627 ) ) ;
#18137 = CARTESIAN_POINT ( 'NONE',  ( 23.49048926389013658, 9.645778135078892035, -218.7307869890797463 ) ) ;
#18138 = CARTESIAN_POINT ( 'NONE',  ( -7.007669255080013926, -23.60960382150139836, -233.3096631214588115 ) ) ;
#18139 = CARTESIAN_POINT ( 'NONE',  ( 18.76166303929371537, 3.000000000000002665, -224.9999999999997442 ) ) ;
#18140 = CARTESIAN_POINT ( 'NONE',  ( -17.78731991475362406, 16.78509880370027929, -218.2387321183659310 ) ) ;
#18141 = FILL_AREA_STYLE ('',( #2816 ) ) ;
#18142 = CARTESIAN_POINT ( 'NONE',  ( 20.07985072697885442, -15.33367264652052953, -217.4666949641080294 ) ) ;
#18143 = CARTESIAN_POINT ( 'NONE',  ( 8.321021197036545303, 25.59447019508656140, -228.6184429848799482 ) ) ;
#18144 = CARTESIAN_POINT ( 'NONE',  ( -11.94782396647286049, 8.456988817430419303, -225.5094493096559063 ) ) ;
#18145 = CARTESIAN_POINT ( 'NONE',  ( -26.42613204384124259, 13.88327151024443395, -218.2510073314678323 ) ) ;
#18146 = CARTESIAN_POINT ( 'NONE',  ( -25.33517302999029042, -8.734563104097837538, -228.3677567689655916 ) ) ;
#18147 = CARTESIAN_POINT ( 'NONE',  ( 9.616550234602936342, 9.263684773868845923, -230.4827401731016607 ) ) ;
#18148 = VECTOR ( 'NONE', #5218, 1000.000000000000000 ) ;
#18149 = MECHANICAL_DESIGN_GEOMETRIC_PRESENTATION_REPRESENTATION (  '', ( #18518 ), #7020 ) ;
#18150 = CARTESIAN_POINT ( 'NONE',  ( 0.000000000000000000, 0.000000000000000000, -77.51594804401857175 ) ) ;
#18151 = CARTESIAN_POINT ( 'NONE',  ( -9.601352586650603982, -12.91383303375239322, -233.5046259060385125 ) ) ;
#18152 = CARTESIAN_POINT ( 'NONE',  ( 9.880827190695510964, 24.82036951119805579, -218.1633337467656020 ) ) ;
#18153 = CARTESIAN_POINT ( 'NONE',  ( 26.91963614581376874, 6.107751173605064920, -232.2246916053503298 ) ) ;
#18154 = CARTESIAN_POINT ( 'NONE',  ( -8.316505849089994129, 18.84563905716333210, -217.0138378867507640 ) ) ;
#18155 = CARTESIAN_POINT ( 'NONE',  ( 12.99334571784053338, 27.47142594410712846, -219.5003755906066658 ) ) ;
#18156 = CARTESIAN_POINT ( 'NONE',  ( 1.152695246012044095, -27.06931983241920747, -220.0193874843003528 ) ) ;
#18157 = ADVANCED_FACE ( 'NONE', ( #6023 ), #21433, .F. ) ;
#18158 = VERTEX_POINT ( 'NONE', #6245 ) ;
#18159 = CARTESIAN_POINT ( 'NONE',  ( -1.981531036097845533, -15.05108582582333909, -227.0172948689592829 ) ) ;
#18160 = CARTESIAN_POINT ( 'NONE',  ( 15.42212722119060864, 5.401662248084913465, -220.8333402320903645 ) ) ;
#18161 = CARTESIAN_POINT ( 'NONE',  ( 13.38839277810360429, -5.174145297632733786, -223.8523798909600941 ) ) ;
#18162 = CARTESIAN_POINT ( 'NONE',  ( -26.22594988380878789, -0.1068133454905619700, -219.1167922977186322 ) ) ;
#18163 = CIRCLE ( 'NONE', #7019, 17.50000000000000711 ) ;
#18164 = CARTESIAN_POINT ( 'NONE',  ( -13.60146639818222702, -25.11808310587244009, -230.9974232610874196 ) ) ;
#18165 = AXIS2_PLACEMENT_3D ( 'NONE', #18827, #15243, #8491 ) ;
#18166 = CARTESIAN_POINT ( 'NONE',  ( 12.11771628698343051, 17.56545729485151952, -218.0322663566023493 ) ) ;
#18167 = PRESENTATION_STYLE_ASSIGNMENT (( #11295 ) ) ;
#18168 = CARTESIAN_POINT ( 'NONE',  ( -18.09994298044773942, 1.383435435878707320, -215.7801353739235708 ) ) ;
#18169 = CARTESIAN_POINT ( 'NONE',  ( 4.484811161826725900, 15.38298568785217313, -219.4617573400562662 ) ) ;
#18170 = CARTESIAN_POINT ( 'NONE',  ( -2.612157044224189484, 27.88031182936952135, -224.5292183073761692 ) ) ;
#18171 = CARTESIAN_POINT ( 'NONE',  ( 15.13450096816097634, -26.20215934980152639, -231.3023426574493726 ) ) ;
#18172 = CARTESIAN_POINT ( 'NONE',  ( 17.97920459523930958, 17.43922474653955490, -233.2737719749805763 ) ) ;
#18173 = CARTESIAN_POINT ( 'NONE',  ( -12.69709334397052203, 10.59859500067950400, -221.6107941937004568 ) ) ;
#18174 = CARTESIAN_POINT ( 'NONE',  ( -17.65933056022148762, 0.7424667221540405260, -229.0964312085266386 ) ) ;
#18175 = CARTESIAN_POINT ( 'NONE',  ( -5.805911442544755552, -26.83424102279996504, -229.6222293353685302 ) ) ;
#18176 = CARTESIAN_POINT ( 'NONE',  ( 14.50000000000000000, 0.000000000000000000, 94.00000000000000000 ) ) ;
#18177 = LINE ( 'NONE', #9621, #5087 ) ;
#18178 = CARTESIAN_POINT ( 'NONE',  ( 14.39473142419577023, 15.98257177912839389, -217.4557725731239373 ) ) ;
#18179 = CARTESIAN_POINT ( 'NONE',  ( 19.65870185572374140, -17.77243814521307641, -229.4329728153015253 ) ) ;
#18180 = FACE_OUTER_BOUND ( 'NONE', #20289, .T. ) ;
#18181 = CARTESIAN_POINT ( 'NONE',  ( -6.163092920833200594, -27.00835405423771007, -232.1022292408408987 ) ) ;
#18182 = DIRECTION ( 'NONE',  ( 1.000000000000000000, 0.000000000000000000, 0.000000000000000000 ) ) ;
#18183 = CARTESIAN_POINT ( 'NONE',  ( -5.807479211365208727, 19.77444019604324410, -216.0778658752277863 ) ) ;
#18184 = CARTESIAN_POINT ( 'NONE',  ( -4.531689447889125866, 14.11317536318881416, -231.6806015375303502 ) ) ;
#18185 = VERTEX_POINT ( 'NONE', #4552 ) ;
#18186 = CARTESIAN_POINT ( 'NONE',  ( -11.24282496690421596, 12.44430180464951086, -232.4405891940542404 ) ) ;
#18187 = CARTESIAN_POINT ( 'NONE',  ( -26.09107693309126574, -10.38942742183557399, -230.9365759677854442 ) ) ;
#18188 = CARTESIAN_POINT ( 'NONE',  ( -23.70746030402021631, -7.943882500033654814, -6.109207967854218602 ) ) ;
#18189 = FACE_BOUND ( 'NONE', #1976, .T. ) ;
#18190 = CARTESIAN_POINT ( 'NONE',  ( -7.825349071214003693, 24.14595706726266755, -216.5959661901539732 ) ) ;
#18191 = CARTESIAN_POINT ( 'NONE',  ( -9.601352586650603982, -12.91383303375239322, -233.5046259060385125 ) ) ;
#18192 = CARTESIAN_POINT ( 'NONE',  ( 20.25084204406298127, -10.11176871144018818, -232.7817218064674591 ) ) ;
#18193 = CARTESIAN_POINT ( 'NONE',  ( -24.02434186778878455, 18.57431834865475651, -228.2662945587547370 ) ) ;
#18194 = CARTESIAN_POINT ( 'NONE',  ( -26.41026844077819291, 5.012316129610852933, -233.8406020309487872 ) ) ;
#18195 = CARTESIAN_POINT ( 'NONE',  ( 5.563568780623874943, 21.86458082533069103, -218.6474243140849012 ) ) ;
#18196 = DIRECTION ( 'NONE',  ( 0.000000000000000000, 0.000000000000000000, -1.000000000000000000 ) ) ;
#18197 = CARTESIAN_POINT ( 'NONE',  ( -17.17143024911216287, 2.756036084795755681, -233.9491886983466316 ) ) ;
#18198 = CARTESIAN_POINT ( 'NONE',  ( -6.911745780724915633, -15.37483479843349699, -221.7918796665217656 ) ) ;
#18199 =( GEOMETRIC_REPRESENTATION_CONTEXT ( 3 ) GLOBAL_UNCERTAINTY_ASSIGNED_CONTEXT ( ( #3109 ) ) GLOBAL_UNIT_ASSIGNED_CONTEXT ( ( #15845, #12472, #15956 ) ) REPRESENTATION_CONTEXT ( 'NONE', 'WORKASPACE' ) );
#18200 = EDGE_CURVE ( 'NONE', #161, #15629, #2312, .T. ) ;
#18201 = ORIENTED_EDGE ( 'NONE', *, *, #861, .F. ) ;
#18202 = CARTESIAN_POINT ( 'NONE',  ( -14.24491355791863612, 5.286533920242113105, -221.7104936369346433 ) ) ;
#18203 = CARTESIAN_POINT ( 'NONE',  ( 10.40160332990717151, 27.59713857063802323, -221.5374724512453213 ) ) ;
#18204 = CARTESIAN_POINT ( 'NONE',  ( -3.162425552858488143, 20.40327580806445695, -216.0004724541873316 ) ) ;
#18205 = ORIENTED_EDGE ( 'NONE', *, *, #704, .T. ) ;
#18206 = CARTESIAN_POINT ( 'NONE',  ( 19.75516891782859474, -3.344025276999063934, -216.3638920815759263 ) ) ;
#18207 = PLANE ( 'NONE',  #660 ) ;
#18208 = ORIENTED_EDGE ( 'NONE', *, *, #15523, .F. ) ;
#18209 = CARTESIAN_POINT ( 'NONE',  ( -11.67631226053870996, 6.737291529340801333, -227.3110382950315227 ) ) ;
#18210 = CARTESIAN_POINT ( 'NONE',  ( -5.579930056231209967, -28.86398153493815144, -221.8494056429758814 ) ) ;
#18211 = CARTESIAN_POINT ( 'NONE',  ( 0.000000000000000000, 0.000000000000000000, -65.00000000000000000 ) ) ;
#18212 = CARTESIAN_POINT ( 'NONE',  ( 7.168644370073567806, 19.32044210858112265, -233.1278450877711634 ) ) ;
#18213 = CARTESIAN_POINT ( 'NONE',  ( 14.72896495958249830, -2.932656333180209796, -224.3388645783988125 ) ) ;
#18214 = EDGE_CURVE ( 'NONE', #1152, #21209, #14525, .T. ) ;
#18215 = CARTESIAN_POINT ( 'NONE',  ( -21.28804099221702018, -0.9277163183344186992, -219.0000000002572733 ) ) ;
#18216 = CARTESIAN_POINT ( 'NONE',  ( 25.02650711521362936, 17.58144575069911042, -223.6165279156031431 ) ) ;
#18217 =( NAMED_UNIT ( * ) PLANE_ANGLE_UNIT ( ) SI_UNIT ( $, .RADIAN. ) );
#18218 = CARTESIAN_POINT ( 'NONE',  ( 15.48014850427786548, 1.347595008492685320, -222.3163328437614723 ) ) ;
#18219 = CARTESIAN_POINT ( 'NONE',  ( 17.97843143658897347, 22.12221935793617078, -220.9346589834416079 ) ) ;
#18220 = DIRECTION ( 'NONE',  ( -1.000000000000000000, 0.000000000000000000, -0.000000000000000000 ) ) ;
#18221 = CARTESIAN_POINT ( 'NONE',  ( 16.44812011099018889, -8.334251478664654655, -229.6488175962812761 ) ) ;
#18222 = CARTESIAN_POINT ( 'NONE',  ( -21.08965452150356867, -10.66825825602615296, -217.1903588586143314 ) ) ;
#18223 = CARTESIAN_POINT ( 'NONE',  ( -22.24611232821838058, -5.847058217106408939, -8.118985252087330906 ) ) ;
#18224 = CARTESIAN_POINT ( 'NONE',  ( 0.000000000000000000, 0.000000000000000000, -60.00000000000000000 ) ) ;
#18225 = CARTESIAN_POINT ( 'NONE',  ( -6.331039912586185814, 17.62337457105953220, -233.2305561356360499 ) ) ;
#18226 = CARTESIAN_POINT ( 'NONE',  ( 12.82249318900957391, -5.922664226158099510, -218.4318038749311768 ) ) ;
#18227 = CARTESIAN_POINT ( 'NONE',  ( 16.06750045776299629, -1.909440863493336860, -220.4398626676318713 ) ) ;
#18228 = CARTESIAN_POINT ( 'NONE',  ( -14.94667331530454213, 6.325011500478772142, -230.0242139990887154 ) ) ;
#18229 = CARTESIAN_POINT ( 'NONE',  ( 12.93042813863272755, 0.4488092930645843914, -225.5263188864764174 ) ) ;
#18230 = CARTESIAN_POINT ( 'NONE',  ( 19.67070349224072956, 16.44307963282299312, -220.0378483479504439 ) ) ;
#18231 = EDGE_LOOP ( 'NONE', ( #18970, #11140, #5487, #6822, #10339, #17124 ) ) ;
#18232 = CARTESIAN_POINT ( 'NONE',  ( 9.588041944343061118, -18.04984130968639633, -234.4334306750605776 ) ) ;
#18233 = CARTESIAN_POINT ( 'NONE',  ( -8.999942255032427951, 11.40691176929435535, 93.00000000000001421 ) ) ;
#18234 = CARTESIAN_POINT ( 'NONE',  ( -31.84745724608465522, 5.474219582435353004, -224.7210333253351564 ) ) ;
#18235 = CARTESIAN_POINT ( 'NONE',  ( 3.641537757978871248, 12.43698445400491437, -220.3805014257186485 ) ) ;
#18236 = CARTESIAN_POINT ( 'NONE',  ( -0.8357710952364670876, 15.48480697989137234, -216.9118565312697910 ) ) ;
#18237 = CARTESIAN_POINT ( 'NONE',  ( 26.09199240421564880, -11.03603815124446186, -222.0211821522591435 ) ) ;
#18238 = CARTESIAN_POINT ( 'NONE',  ( -7.189383125363055349, 14.28512618638020548, -231.7475838278701303 ) ) ;
#18239 = FACE_OUTER_BOUND ( 'NONE', #1560, .T. ) ;
#18240 = EDGE_CURVE ( 'NONE', #13837, #3651, #13762, .T. ) ;
#18241 = CARTESIAN_POINT ( 'NONE',  ( 2.804048525646705148, 30.59371477727813726, -220.6614663749232363 ) ) ;
#18242 = CARTESIAN_POINT ( 'NONE',  ( -16.88427011841620029, 9.219900108593305887, -231.9155403335099948 ) ) ;
#18243 = CARTESIAN_POINT ( 'NONE',  ( -9.540790481621398200, 9.981116473660406996, -228.6478862620407995 ) ) ;
#18244 = CARTESIAN_POINT ( 'NONE',  ( 14.73698509926073186, 4.443590625350892331, -227.4062002049096236 ) ) ;
#18245 = CARTESIAN_POINT ( 'NONE',  ( 9.382249691333727881, 26.55946126407900820, -224.4468135941759215 ) ) ;
#18246 = CARTESIAN_POINT ( 'NONE',  ( 0.000000000000000000, 0.000000000000000000, -69.99999999999998579 ) ) ;
#18247 = VERTEX_POINT ( 'NONE', #21379 ) ;
#18248 = CARTESIAN_POINT ( 'NONE',  ( 10.32480721127626033, 15.84468581819879773, -230.0799086455579072 ) ) ;
#18249 = CARTESIAN_POINT ( 'NONE',  ( -21.08965452150356867, -10.66825825602615296, -217.1903588586143314 ) ) ;
#18250 = CARTESIAN_POINT ( 'NONE',  ( 16.00819137755116373, 4.595691552992191120, -229.5669508871464757 ) ) ;
#18251 = CARTESIAN_POINT ( 'NONE',  ( -3.642659482353215239, -13.10753628101701018, -222.6432544668793980 ) ) ;
#18252 = CARTESIAN_POINT ( 'NONE',  ( 0.000000000000000000, 0.000000000000000000, 94.00000000000000000 ) ) ;
#18253 = CARTESIAN_POINT ( 'NONE',  ( -7.284474494690100776, 13.60812129561547046, -227.7414351104868331 ) ) ;
#18254 = CARTESIAN_POINT ( 'NONE',  ( 14.68951511424354273, -18.85605729411972575, -217.5026406474102885 ) ) ;
#18255 = CARTESIAN_POINT ( 'NONE',  ( 11.75069299018312208, 6.043853022588032253, -224.2604610870103841 ) ) ;
#18256 = CARTESIAN_POINT ( 'NONE',  ( -16.57767831947938575, 23.50485984366324388, -222.7977068309636763 ) ) ;
#18257 = CARTESIAN_POINT ( 'NONE',  ( -27.68973657932738064, 5.930811633061950694, -216.7842770206311513 ) ) ;
#18258 = CARTESIAN_POINT ( 'NONE',  ( -13.57658210113775432, -10.11812981318216131, -221.5438341886276987 ) ) ;
#18259 = CARTESIAN_POINT ( 'NONE',  ( 16.53896178738450828, 2.691624496798088462, -232.5974196329879078 ) ) ;
#18260 = FACE_OUTER_BOUND ( 'NONE', #4858, .T. ) ;
#18261 = CARTESIAN_POINT ( 'NONE',  ( -20.50691009226094863, -22.90269851828495007, -230.6242067303112435 ) ) ;
#18262 = CARTESIAN_POINT ( 'NONE',  ( 0.3632086708616291126, 21.06287758167331958, -232.5112839711303820 ) ) ;
#18263 = CARTESIAN_POINT ( 'NONE',  ( -17.72669652144150376, 1.460525322529694581, -220.6883622781615202 ) ) ;
#18264 = CARTESIAN_POINT ( 'NONE',  ( -15.77374768176864173, 20.07639682234129097, -218.6858893794192795 ) ) ;
#18265 = CARTESIAN_POINT ( 'NONE',  ( 7.393167209263542539, 10.77319710117329699, -221.1179833906701049 ) ) ;
#18266 = EDGE_LOOP ( 'NONE', ( #14653, #7522, #5932, #6771, #1569, #15987, #10227 ) ) ;
#18267 = CARTESIAN_POINT ( 'NONE',  ( -5.474373895759362618, -29.29005893717160092, -223.2371403555430334 ) ) ;
#18268 = ORIENTED_EDGE ( 'NONE', *, *, #5782, .F. ) ;
#18269 = CARTESIAN_POINT ( 'NONE',  ( 5.191785474240024456, -25.78595846473334419, -219.2330600099714673 ) ) ;
#18270 = AXIS2_PLACEMENT_3D ( 'NONE', #18534, #1534, #22129 ) ;
#18271 = CARTESIAN_POINT ( 'NONE',  ( -21.73153953336191790, 8.758376218440917071, -235.2971293019126051 ) ) ;
#18272 = CARTESIAN_POINT ( 'NONE',  ( 21.30961698559626427, -20.48616475849644303, -228.5322376518520002 ) ) ;
#18273 = CARTESIAN_POINT ( 'NONE',  ( -23.10791503177032880, -5.282985115830100220, -217.6364121950018671 ) ) ;
#18274 = CARTESIAN_POINT ( 'NONE',  ( -8.514447835183077018, -10.26590951297754195, -225.5321622820681569 ) ) ;
#18275 = CARTESIAN_POINT ( 'NONE',  ( 14.87635807518583775, 11.13002414557121789, -232.1789382499626981 ) ) ;
#18276 = CARTESIAN_POINT ( 'NONE',  ( 0.000000000000000000, 17.50000000000000711, -55.00000000000000000 ) ) ;
#18277 = CARTESIAN_POINT ( 'NONE',  ( -12.33997807949817904, 15.01940705987184188, -217.6798968600957380 ) ) ;
#18278 = CARTESIAN_POINT ( 'NONE',  ( 1.773982976645536835, 19.12448993322812285, -233.2315972735944172 ) ) ;
#18279 = CARTESIAN_POINT ( 'NONE',  ( 11.39755372583812587, 20.40856199875060639, -231.2895618162029621 ) ) ;
#18280 = CARTESIAN_POINT ( 'NONE',  ( 22.52555938611480002, -22.70209057424856525, -227.7033606670069332 ) ) ;
#18281 = CARTESIAN_POINT ( 'NONE',  ( 10.12956299421491302, 11.38773431477224385, -230.3175791991728829 ) ) ;
#18282 = CARTESIAN_POINT ( 'NONE',  ( -16.58624905143161143, 8.715293938925766426, -220.0618460037763384 ) ) ;
#18283 = CARTESIAN_POINT ( 'NONE',  ( 1.366658787427950772, -15.59113167952139456, -228.2894046839634257 ) ) ;
#18284 = CARTESIAN_POINT ( 'NONE',  ( -16.20072894238734307, 0.5024448614660336210, -230.4554067149722130 ) ) ;
#18285 = FACE_OUTER_BOUND ( 'NONE', #14033, .T. ) ;
#18286 = CARTESIAN_POINT ( 'NONE',  ( 21.25094435758043332, 17.68230636442804027, -229.7964888993842010 ) ) ;
#18287 = CARTESIAN_POINT ( 'NONE',  ( 12.89329787743523070, -9.350464391519500040, -225.0861735818250224 ) ) ;
#18288 = ADVANCED_FACE ( 'NONE', ( #4608 ), #16113, .T. ) ;
#18289 = CARTESIAN_POINT ( 'NONE',  ( -24.63401512838757768, 0.000000000000000000, 77.51594804401857175 ) ) ;
#18290 = AXIS2_PLACEMENT_3D ( 'NONE', #15751, #1891, #17654 ) ;
#18291 = CARTESIAN_POINT ( 'NONE',  ( -9.606889355748592152, -11.26588727105406385, -229.9123324032181586 ) ) ;
#18292 = CARTESIAN_POINT ( 'NONE',  ( 0.2389779871941385414, 16.64595486589868045, -218.1658233406367629 ) ) ;
#18293 = CARTESIAN_POINT ( 'NONE',  ( 3.764125772070460396, 11.78312483992801596, -228.3484643988637970 ) ) ;
#18294 = ORIENTED_EDGE ( 'NONE', *, *, #13698, .T. ) ;
#18295 = CARTESIAN_POINT ( 'NONE',  ( -0.9414827276148034496, 23.96885519606619752, -216.4491898092606164 ) ) ;
#18296 = CARTESIAN_POINT ( 'NONE',  ( -28.57583275380518018, -9.842401781236429059, -222.4643230566485386 ) ) ;
#18297 = CARTESIAN_POINT ( 'NONE',  ( -24.30915884321608544, -5.843097688897257669, -8.121843009851255957 ) ) ;
#18298 = CARTESIAN_POINT ( 'NONE',  ( 2.999999999999975131, 3.673940397442062826E-16, -105.0000000000000142 ) ) ;
#18299 = CARTESIAN_POINT ( 'NONE',  ( -2.208416658185406334, 29.10348627872611615, -219.8480645685746424 ) ) ;
#18300 = CARTESIAN_POINT ( 'NONE',  ( -4.398080837965281376, -27.92536303359771566, -232.3360949592949112 ) ) ;
#18301 = CARTESIAN_POINT ( 'NONE',  ( 24.80560757033128993, -15.22139526172250079, -221.3338856610240271 ) ) ;
#18302 = CARTESIAN_POINT ( 'NONE',  ( -3.755296588130283553, 23.77975947300719284, -233.7323173085780752 ) ) ;
#18303 = CARTESIAN_POINT ( 'NONE',  ( -24.79170285622992509, 4.551775110860766915, -234.5907228154019322 ) ) ;
#18304 = CARTESIAN_POINT ( 'NONE',  ( 3.755480357635514022, 24.23367984900377436, -231.4105847235276201 ) ) ;
#18305 = DIRECTION ( 'NONE',  ( 1.000000000000000000, 0.000000000000000000, 0.000000000000000000 ) ) ;
#18306 = CARTESIAN_POINT ( 'NONE',  ( 14.32363442937021425, 2.978337679677412808, -227.0386046113487453 ) ) ;
#18307 = CARTESIAN_POINT ( 'NONE',  ( -21.61315260466662380, -9.974349528768403417, -231.2583083768228960 ) ) ;
#18308 = ORIENTED_EDGE ( 'NONE', *, *, #5288, .F. ) ;
#18309 = CARTESIAN_POINT ( 'NONE',  ( -14.94640692938030746, 5.382918922058764544, -220.5478552936960455 ) ) ;
#18310 = CARTESIAN_POINT ( 'NONE',  ( 2.471164685565028662, 14.01327037412690935, -223.4905256513065410 ) ) ;
#18311 = CARTESIAN_POINT ( 'NONE',  ( -5.562203253303141359, 12.75725363875033302, -225.3078268727488478 ) ) ;
#18312 = CARTESIAN_POINT ( 'NONE',  ( -14.97948828349161232, -4.621108923465524931, -227.6270126398174796 ) ) ;
#18313 = CARTESIAN_POINT ( 'NONE',  ( 1.322875655532295358, 1.500000000000000000, -378.2244600276337678 ) ) ;
#18314 = EDGE_LOOP ( 'NONE', ( #9096, #6748, #9360, #20921 ) ) ;
#18315 = CARTESIAN_POINT ( 'NONE',  ( -13.83274569775339202, 16.20364235096346661, -234.0851861771356539 ) ) ;
#18316 = CARTESIAN_POINT ( 'NONE',  ( -19.49800774256867086, -24.03546784425654792, -228.3621204403185061 ) ) ;
#18317 = CARTESIAN_POINT ( 'NONE',  ( 14.80138866163881772, 1.641909370019589032, -227.5118825796487272 ) ) ;
#18318 = CARTESIAN_POINT ( 'NONE',  ( 13.43170911749896490, 19.07691563292472026, -232.7497845103644636 ) ) ;
#18319 = CARTESIAN_POINT ( 'NONE',  ( -21.50000000000001066, 0.000000000000000000, -30.00000000000000000 ) ) ;
#18320 = DIRECTION ( 'NONE',  ( 0.000000000000000000, 0.000000000000000000, 1.000000000000000000 ) ) ;
#18321 = CARTESIAN_POINT ( 'NONE',  ( -13.01696012539752445, 9.878799299062107409, -218.8446158128127195 ) ) ;
#18322 = EDGE_CURVE ( 'NONE', #4932, #2027, #16832, .T. ) ;
#18323 = CARTESIAN_POINT ( 'NONE',  ( 13.14260364752544596, 5.866423290307341887, -222.7705901084601408 ) ) ;
#18324 = DIRECTION ( 'NONE',  ( 0.000000000000000000, 0.000000000000000000, 1.000000000000000000 ) ) ;
#18325 = CARTESIAN_POINT ( 'NONE',  ( 15.61962121506769385, 4.525360868525488911, -229.0684696061408090 ) ) ;
#18326 = CARTESIAN_POINT ( 'NONE',  ( -3.400000000000003908, 0.000000000000000000, -224.9999999999999716 ) ) ;
#18327 = CARTESIAN_POINT ( 'NONE',  ( 16.03897629125586377, -3.546747291816754633, -223.1229430630804700 ) ) ;
#18328 = CARTESIAN_POINT ( 'NONE',  ( -22.53818779203657741, -7.663114047788936567, -232.6164956747681458 ) ) ;
#18329 = CARTESIAN_POINT ( 'NONE',  ( 0.000000000000000000, -23.00000000000000000, 75.00000000000000000 ) ) ;
#18330 = DIRECTION ( 'NONE',  ( -1.000000000000000000, -0.000000000000000000, -0.000000000000000000 ) ) ;
#18331 = CARTESIAN_POINT ( 'NONE',  ( -4.558896566524145655, 13.01459016691503301, -228.3167740496058684 ) ) ;
#18332 = CARTESIAN_POINT ( 'NONE',  ( 30.90240445905660138, -9.617167762261830788, -225.5262352394493064 ) ) ;
#18333 = CARTESIAN_POINT ( 'NONE',  ( 28.36095019830170472, -8.296631283839911220, -225.2861439608085448 ) ) ;
#18334 = CARTESIAN_POINT ( 'NONE',  ( -15.82622499106666325, 9.895986579907866343, -218.5115209877527604 ) ) ;
#18335 = CARTESIAN_POINT ( 'NONE',  ( 13.19406830060760605, 4.163358546877222288, -228.8532745215267425 ) ) ;
#18336 = CARTESIAN_POINT ( 'NONE',  ( 24.93482953594869755, 13.13888391581411241, -222.4369546851285691 ) ) ;
#18337 = CARTESIAN_POINT ( 'NONE',  ( 3.813635332914135923, -14.61080527247722927, -220.2619188551939828 ) ) ;
#18338 = CARTESIAN_POINT ( 'NONE',  ( 18.54610009393809023, 0.6523581019769808531, -231.1787333216317677 ) ) ;
#18339 = CARTESIAN_POINT ( 'NONE',  ( -10.54177647804913320, 7.401649028325941515, -220.3980514230326264 ) ) ;
#18340 = CARTESIAN_POINT ( 'NONE',  ( 12.90536070039565963, 17.66816134723717724, -234.8562535614228750 ) ) ;
#18341 = CARTESIAN_POINT ( 'NONE',  ( 2.660414182604129429, 28.99288898680367055, -232.5781547115647072 ) ) ;
#18342 = CARTESIAN_POINT ( 'NONE',  ( 14.50342097185254353, -4.720444175079822280, -222.5922120714632513 ) ) ;
#18343 = CARTESIAN_POINT ( 'NONE',  ( -1.881996891245037995, 28.05344686410985489, -218.6379207300106202 ) ) ;
#18344 = CARTESIAN_POINT ( 'NONE',  ( -21.93900267957129557, 7.862893636934532360, -233.4951761057262161 ) ) ;
#18345 = CARTESIAN_POINT ( 'NONE',  ( 18.15173157547545557, 23.32481284044927961, -217.8532150843729482 ) ) ;
#18346 = CARTESIAN_POINT ( 'NONE',  ( -18.88344489807484905, 1.071113352238720617, -230.0966926586188208 ) ) ;
#18347 = CARTESIAN_POINT ( 'NONE',  ( -13.55591840520136770, 8.363404288414606924, -231.2690188357804857 ) ) ;
#18348 = CARTESIAN_POINT ( 'NONE',  ( 27.75679124201660741, 4.911524026080384075, -221.4430403652340829 ) ) ;
#18349 = CARTESIAN_POINT ( 'NONE',  ( 7.804112641607792611, 19.76858558208418515, -218.6463059509973164 ) ) ;
#18350 = CARTESIAN_POINT ( 'NONE',  ( 15.58663895521930876, 0.3114376099562851108, -227.9849797934280957 ) ) ;
#18351 = LINE ( 'NONE', #19389, #10597 ) ;
#18352 = CARTESIAN_POINT ( 'NONE',  ( 10.89019654021101857, 23.08162452736882031, -220.1893104909416934 ) ) ;
#18353 = CARTESIAN_POINT ( 'NONE',  ( -21.28605893225895684, -20.43870967537180050, -221.0356759888913700 ) ) ;
#18354 = CARTESIAN_POINT ( 'NONE',  ( 14.19800769603076240, 4.587407146151301518, -224.2928935459285071 ) ) ;
#18355 = CARTESIAN_POINT ( 'NONE',  ( -8.609577223708431148, -18.69066821291321290, -217.1995118692595099 ) ) ;
#18356 = DIRECTION ( 'NONE',  ( 1.000000000000000000, 0.000000000000000000, 0.000000000000000000 ) ) ;
#18357 = CARTESIAN_POINT ( 'NONE',  ( -4.490213599459100813, 14.55066867058898694, -222.6488251579668827 ) ) ;
#18358 =( LENGTH_UNIT ( ) NAMED_UNIT ( * ) SI_UNIT ( .MILLI., .METRE. ) );
#18359 = CARTESIAN_POINT ( 'NONE',  ( 15.50624253654579654, -15.96056326703506478, -233.0338314371582840 ) ) ;
#18360 = EDGE_CURVE ( 'NONE', #8526, #8590, #16219, .T. ) ;
#18361 = CARTESIAN_POINT ( 'NONE',  ( 12.14863411169100971, 10.95505907656739097, -219.3725293661985063 ) ) ;
#18362 = CARTESIAN_POINT ( 'NONE',  ( -10.91003322996498071, 12.84665145358222382, -229.9786893781767958 ) ) ;
#18363 = CARTESIAN_POINT ( 'NONE',  ( -20.06846544527470400, 7.877362284741439069, -235.3910773253824402 ) ) ;
#18364 = CARTESIAN_POINT ( 'NONE',  ( -14.79915263310685347, -6.493660518011266092, -224.0818296219458716 ) ) ;
#18365 = EDGE_CURVE ( 'NONE', #14027, #2064, #12952, .T. ) ;
#18366 = CARTESIAN_POINT ( 'NONE',  ( -24.49083850720273148, 4.222094140707651100, -219.1543001448025905 ) ) ;
#18367 = DIRECTION ( 'NONE',  ( 6.123233995736766036E-17, -0.000000000000000000, -1.000000000000000000 ) ) ;
#18368 = CARTESIAN_POINT ( 'NONE',  ( -24.78158512205813224, 1.917202307505101455, -217.2232489266994833 ) ) ;
#18369 = CARTESIAN_POINT ( 'NONE',  ( 14.63115627273841923, 9.024791562541032874, -232.5054678133655841 ) ) ;
#18370 = CARTESIAN_POINT ( 'NONE',  ( -16.03353370602922467, 4.897644413504528060, -222.5335369890782999 ) ) ;
#18371 = CARTESIAN_POINT ( 'NONE',  ( 2.987882271643250931, 28.57355997650491020, -217.8917278841813925 ) ) ;
#18372 = CARTESIAN_POINT ( 'NONE',  ( 20.05374812456133782, 24.17492691056345677, -223.1494843338164458 ) ) ;
#18373 = CARTESIAN_POINT ( 'NONE',  ( -11.90549671174648694, -23.44716645851259784, -216.8989558407570257 ) ) ;
#18374 = EDGE_LOOP ( 'NONE', ( #8995, #9538, #7440, #3344 ) ) ;
#18375 = CARTESIAN_POINT ( 'NONE',  ( 6.930886114109415352, -28.33506752827666020, -226.0544877841801110 ) ) ;
#18376 = CARTESIAN_POINT ( 'NONE',  ( -16.85225081326727903, 6.237400186851330020, -234.5847093771173206 ) ) ;
#18377 = CARTESIAN_POINT ( 'NONE',  ( 19.06212547406409641, -9.287000003594721775, -232.7453815625877667 ) ) ;
#18378 = CARTESIAN_POINT ( 'NONE',  ( 29.31647908907816102, 0.9594737942742700421, -228.5782466420670858 ) ) ;
#18379 = ADVANCED_FACE ( 'NONE', ( #6303 ), #5855, .F. ) ;
#18380 = CARTESIAN_POINT ( 'NONE',  ( -15.48425879135615446, -25.29886615046042309, -220.6886037686364261 ) ) ;
#18381 = CARTESIAN_POINT ( 'NONE',  ( 10.49810582199713416, 9.357428619962972149, -224.5466107281195605 ) ) ;
#18382 = CARTESIAN_POINT ( 'NONE',  ( -21.00000000000000000, 0.000000000000000000, 75.00000000000000000 ) ) ;
#18383 = CARTESIAN_POINT ( 'NONE',  ( -8.112279890008961658, 11.99566605360304727, -225.9834628568286519 ) ) ;
#18384 = CARTESIAN_POINT ( 'NONE',  ( 11.41090957555148222, 16.52772439454343711, -218.2458222691329013 ) ) ;
#18385 = CARTESIAN_POINT ( 'NONE',  ( 4.907833106823921376, 13.98151846258800290, -229.0190609869640923 ) ) ;
#18386 = CARTESIAN_POINT ( 'NONE',  ( 19.61276001257277102, 19.97122404150989894, -229.5162757829903342 ) ) ;
#18387 = CARTESIAN_POINT ( 'NONE',  ( 26.60633779560760459, -14.33430814915920593, -230.5388497754989885 ) ) ;
#18388 = CARTESIAN_POINT ( 'NONE',  ( 20.05202556141620107, 8.012988804822112954, -215.8722494878839200 ) ) ;
#18389 = CARTESIAN_POINT ( 'NONE',  ( -9.007976471255481954, 12.60968992764439633, -227.9367755778692981 ) ) ;
#18390 = CARTESIAN_POINT ( 'NONE',  ( -10.06927776881013514, -17.00317020600589402, -217.8513858272130790 ) ) ;
#18391 = DIRECTION ( 'NONE',  ( 0.000000000000000000, 0.000000000000000000, -1.000000000000000000 ) ) ;
#18392 = CARTESIAN_POINT ( 'NONE',  ( 25.50000000000000000, 4.399999999999999467, -3.300000000000000266 ) ) ;
#18393 = CIRCLE ( 'NONE', #13364, 23.00000000000008882 ) ;
#18394 = CARTESIAN_POINT ( 'NONE',  ( 13.43730899468209294, 8.427513769504761498, -221.4030804848920297 ) ) ;
#18395 = CARTESIAN_POINT ( 'NONE',  ( 9.552164729858477088, -28.54380927792562872, -224.2925619065192677 ) ) ;
#18396 = CARTESIAN_POINT ( 'NONE',  ( -14.24491355791863612, 5.286533920242113105, -221.7104936369346433 ) ) ;
#18397 = CARTESIAN_POINT ( 'NONE',  ( -14.24095617957673632, -25.86326826095433162, -229.7068514753157160 ) ) ;
#18398 = ITEM_DEFINED_TRANSFORMATION ( 'NONE', 'NONE', #15648,  #6677 ) ;
#18399 = CARTESIAN_POINT ( 'NONE',  ( 15.96089671440110713, 1.143943728337336374, -218.3532651118343892 ) ) ;
#18400 = ADVANCED_FACE ( 'NONE', ( #7674 ), #20189, .F. ) ;
#18401 = AXIS2_PLACEMENT_3D ( 'NONE', #14796, #15134, #12989 ) ;
#18402 = CARTESIAN_POINT ( 'NONE',  ( -4.619644865335168049, 14.75104250038670450, -232.3086264397671812 ) ) ;
#18403 = ORIENTED_EDGE ( 'NONE', *, *, #7416, .F. ) ;
#18404 = CARTESIAN_POINT ( 'NONE',  ( -2.808235066048971440, 30.42019778760651150, -222.6481917607299295 ) ) ;
#18405 = CARTESIAN_POINT ( 'NONE',  ( -18.41550138691291139, -5.273244084890690075, -216.7348800533310964 ) ) ;
#18406 = CARTESIAN_POINT ( 'NONE',  ( -24.49471200173250907, -5.031606206670845793, -8.666454690105759084 ) ) ;
#18407 = CARTESIAN_POINT ( 'NONE',  ( -2.775557561562891351E-14, 0.000000000000000000, -105.0000000000000142 ) ) ;
#18408 = CARTESIAN_POINT ( 'NONE',  ( -3.368164009525018265, 19.03203264544105622, -233.5986411977714567 ) ) ;
#18409 = CARTESIAN_POINT ( 'NONE',  ( -6.645226799955220365, -27.24439832571371767, -217.1032720093393493 ) ) ;
#18410 = CARTESIAN_POINT ( 'NONE',  ( 8.332496243628455090, -29.79192972398156769, -226.1452587264855367 ) ) ;
#18411 = DIRECTION ( 'NONE',  ( 1.000000000000000000, 0.000000000000000000, 0.000000000000000000 ) ) ;
#18412 = AXIS2_PLACEMENT_3D ( 'NONE', #1865, #8746, #19079 ) ;
#18413 = CARTESIAN_POINT ( 'NONE',  ( -11.11821474075380678, 16.53100589793018926, -232.3736596382188395 ) ) ;
#18414 = CARTESIAN_POINT ( 'NONE',  ( 8.162622027327667951, 13.88735946031204094, -224.7165241036068153 ) ) ;
#18415 = CARTESIAN_POINT ( 'NONE',  ( -18.46722752239034193, 0.9784074152395518809, -232.1633353206286188 ) ) ;
#18416 = CARTESIAN_POINT ( 'NONE',  ( -17.07051451008491938, 15.19890664381897949, -233.6014043774825666 ) ) ;
#18417 = CARTESIAN_POINT ( 'NONE',  ( -26.24201160508392761, -9.884581200937399004, -221.6903139798603206 ) ) ;
#18418 = CARTESIAN_POINT ( 'NONE',  ( -14.22255565734842619, 21.32307452572284134, -218.8849463683180261 ) ) ;
#18419 = CARTESIAN_POINT ( 'NONE',  ( 20.05202556141620107, 8.012988804822112954, -215.8722494878839200 ) ) ;
#18420 = CARTESIAN_POINT ( 'NONE',  ( 2.631948090663005946, 31.21493676147814611, -222.3107766067421380 ) ) ;
#18421 = CARTESIAN_POINT ( 'NONE',  ( 11.81564506561547390, -6.597897255275705142, -225.1493936678799628 ) ) ;
#18422 = DIRECTION ( 'NONE',  ( 0.000000000000000000, 0.000000000000000000, 1.000000000000000000 ) ) ;
#18423 = ORIENTED_EDGE ( 'NONE', *, *, #6211, .F. ) ;
#18424 = CARTESIAN_POINT ( 'NONE',  ( -9.540790481621398200, 9.981116473660406996, -228.6478862620407995 ) ) ;
#18425 = CARTESIAN_POINT ( 'NONE',  ( -12.75534255189586652, -28.05386989040209400, -226.4018635127162327 ) ) ;
#18426 = CARTESIAN_POINT ( 'NONE',  ( 17.34727976380017722, 4.822939981779328811, -230.8836217450937909 ) ) ;
#18427 = CARTESIAN_POINT ( 'NONE',  ( 7.743212835174657194, 11.90778931056080481, -226.0491028376908105 ) ) ;
#18428 = DIRECTION ( 'NONE',  ( -1.083936797661037871E-15, -1.000000000000000000, 0.000000000000000000 ) ) ;
#18429 = UNCERTAINTY_MEASURE_WITH_UNIT (LENGTH_MEASURE( 1.000000000000000082E-05 ), #3111, 'distance_accuracy_value', 'NONE');
#18430 = DIRECTION ( 'NONE',  ( 1.000000000000000000, 0.000000000000000000, 0.000000000000000000 ) ) ;
#18431 = CARTESIAN_POINT ( 'NONE',  ( -22.57859951143173660, 16.82392524473188899, -219.5628058978911383 ) ) ;
#18432 = AXIS2_PLACEMENT_3D ( 'NONE', #14230, #17822, #12304 ) ;
#18433 = EDGE_CURVE ( 'NONE', #6505, #14565, #10508, .T. ) ;
#18434 = CARTESIAN_POINT ( 'NONE',  ( 15.07212457412616224, 2.472408313530222390, -227.3472192494155024 ) ) ;
#18435 = VECTOR ( 'NONE', #14410, 1000.000000000000000 ) ;
#18436 = CARTESIAN_POINT ( 'NONE',  ( 14.86622134549281427, 0.1848946639127413416, -222.0051228238385477 ) ) ;
#18437 = CARTESIAN_POINT ( 'NONE',  ( 19.20300624114736721, 0.6066039755357417462, -231.5046416827383950 ) ) ;
#18438 = CARTESIAN_POINT ( 'NONE',  ( -17.96792326766206926, -0.6237852504629022299, -217.9759415197746932 ) ) ;
#18439 = CARTESIAN_POINT ( 'NONE',  ( 19.48258831087540344, -3.612136468958778934, -219.4255404790470436 ) ) ;
#18440 = CARTESIAN_POINT ( 'NONE',  ( -14.37894460687751597, -1.926260335694933268, -225.0161641904981593 ) ) ;
#18441 = CARTESIAN_POINT ( 'NONE',  ( -20.83650439078820682, -9.738852918555068072, -2.294278442558280506 ) ) ;
#18442 = DIRECTION ( 'NONE',  ( 0.000000000000000000, 0.000000000000000000, -1.000000000000000000 ) ) ;
#18443 = CARTESIAN_POINT ( 'NONE',  ( 6.685304925496912354, 17.61973327427626046, -230.4152170797364931 ) ) ;
#18444 = CARTESIAN_POINT ( 'NONE',  ( 8.773758653197093693, -22.96626044227292951, -216.4280442219689178 ) ) ;
#18445 = CARTESIAN_POINT ( 'NONE',  ( 12.84024077373997841, -14.50125846907313054, -216.8496453050001946 ) ) ;
#18446 = CARTESIAN_POINT ( 'NONE',  ( -15.83178333309709629, 2.467763724635483324, -230.4064772870105458 ) ) ;
#18447 = CARTESIAN_POINT ( 'NONE',  ( 13.16746181015946959, 0.3897807143096829741, -227.1676274388083243 ) ) ;
#18448 = CARTESIAN_POINT ( 'NONE',  ( 17.42772712443221650, 11.35756022693713341, -231.2166398222404382 ) ) ;
#18449 = CARTESIAN_POINT ( 'NONE',  ( 2.859576749041432553, -13.55982619688326984, -227.5954719880151345 ) ) ;
#18450 = CARTESIAN_POINT ( 'NONE',  ( -2.465190328815661892E-29, -25.00000000000012790, 75.00000000000000000 ) ) ;
#18451 = AXIS2_PLACEMENT_3D ( 'NONE', #7227, #8914, #5519 ) ;
#18452 = CARTESIAN_POINT ( 'NONE',  ( -24.77996431573922820, 10.49354383977773786, -234.1655613096203581 ) ) ;
#18453 = CIRCLE ( 'NONE', #1570, 25.00000000000000000 ) ;
#18454 = CARTESIAN_POINT ( 'NONE',  ( 11.84598249547323690, 10.36127485500543699, -218.5481300776139904 ) ) ;
#18455 = CARTESIAN_POINT ( 'NONE',  ( 3.744112528862662881, 31.76296354843916703, -227.8872370379487506 ) ) ;
#18456 = CARTESIAN_POINT ( 'NONE',  ( 16.71284463105542883, -8.832875790685479345, -219.1937169315102949 ) ) ;
#18457 = CARTESIAN_POINT ( 'NONE',  ( -8.966714183099560032, 19.05224306381768073, -234.0879867025980445 ) ) ;
#18458 = CARTESIAN_POINT ( 'NONE',  ( -25.80904414196669450, 12.19501778665756220, -219.1732313092283846 ) ) ;
#18459 = CARTESIAN_POINT ( 'NONE',  ( 9.986779374595107228, 29.47523823012521049, -229.5287702428778687 ) ) ;
#18460 = CARTESIAN_POINT ( 'NONE',  ( -20.95553895916151177, 12.88782924195037438, -232.2493899712447956 ) ) ;
#18461 = CARTESIAN_POINT ( 'NONE',  ( -3.205260335674071648, 17.52234722004434531, -232.9754319808710363 ) ) ;
#18462 = CARTESIAN_POINT ( 'NONE',  ( -1.509788170712026423, 10.75822951548914830, 91.99999999999998579 ) ) ;
#18463 = VECTOR ( 'NONE', #17445, 1000.000000000000000 ) ;
#18464 = CARTESIAN_POINT ( 'NONE',  ( 3.174664235197445006, 17.30896320251298448, -221.0803896709622620 ) ) ;
#18465 = AXIS2_PLACEMENT_3D ( 'NONE', #15074, #10002, #18880 ) ;
#18466 = CARTESIAN_POINT ( 'NONE',  ( 27.92729748684602598, -8.572309054117944527, -222.6487661343338686 ) ) ;
#18467 = DIRECTION ( 'NONE',  ( -1.000000000000000000, 0.000000000000000000, 0.000000000000000000 ) ) ;
#18468 = DIRECTION ( 'NONE',  ( 1.000000000000000000, -1.083936797661038068E-15, 0.000000000000000000 ) ) ;
#18469 = CARTESIAN_POINT ( 'NONE',  ( 20.34032485158648029, 2.741617426884598530, -217.9827731991294968 ) ) ;
#18470 = CARTESIAN_POINT ( 'NONE',  ( -10.89162261547930655, -11.18732543557264592, -227.7569336215896953 ) ) ;
#18471 = CARTESIAN_POINT ( 'NONE',  ( 19.24993070808566387, 2.578473320807614488, -226.5486764295067417 ) ) ;
#18472 = CARTESIAN_POINT ( 'NONE',  ( -4.073886805163430935, 14.35067061637828623, -226.4733297826468572 ) ) ;
#18473 = CARTESIAN_POINT ( 'NONE',  ( 14.46917091355089902, -8.493370822347547033, -231.7163745456035997 ) ) ;
#18474 = CARTESIAN_POINT ( 'NONE',  ( 21.24820809707834357, 20.59746639607275398, -225.8540969741923732 ) ) ;
#18475 = CARTESIAN_POINT ( 'NONE',  ( -16.50467377682197423, 21.56569464670658220, -229.9175202103629374 ) ) ;
#18476 = CARTESIAN_POINT ( 'NONE',  ( -9.045741320599788082, 11.46901338045063312, -219.0588111342715365 ) ) ;
#18477 = ORIENTED_EDGE ( 'NONE', *, *, #7604, .F. ) ;
#18478 = CARTESIAN_POINT ( 'NONE',  ( -13.39502153392024475, -9.880902914596246589, -222.0112808355889342 ) ) ;
#18479 = EDGE_CURVE ( 'NONE', #20995, #19105, #9442, .T. ) ;
#18480 = CARTESIAN_POINT ( 'NONE',  ( -17.59913672443795463, -0.5356773789333074687, -220.7342471185320960 ) ) ;
#18481 = DIRECTION ( 'NONE',  ( -1.000000000000000000, 0.000000000000000000, 0.000000000000000000 ) ) ;
#18482 = CARTESIAN_POINT ( 'NONE',  ( -22.30463520409893263, -0.6981587008078518064, -233.9491726243120127 ) ) ;
#18483 = CARTESIAN_POINT ( 'NONE',  ( 21.38922145650625239, 17.10616209967719215, -217.8354246241890451 ) ) ;
#18484 = TOROIDAL_SURFACE ( 'NONE', #7029, 24.63401512838747820, 3.000000000000000888 ) ;
#18485 = CARTESIAN_POINT ( 'NONE',  ( -17.64438593497130370, 2.824953307685432069, -229.4443205246391813 ) ) ;
#18486 = CARTESIAN_POINT ( 'NONE',  ( 11.20713200305815427, 28.28922876448651635, -219.1239564724620834 ) ) ;
#18487 = ADVANCED_FACE ( 'NONE', ( #16548 ), #21711, .T. ) ;
#18488 = CARTESIAN_POINT ( 'NONE',  ( 25.60482246989237609, 8.614967517510873307, -219.3103232513597618 ) ) ;
#18489 = ORIENTED_EDGE ( 'NONE', *, *, #4731, .T. ) ;
#18490 = CARTESIAN_POINT ( 'NONE',  ( -8.763358281418030415, -9.103836352148345412, -222.0692104753270257 ) ) ;
#18491 = ORIENTED_EDGE ( 'NONE', *, *, #12993, .F. ) ;
#18492 = CARTESIAN_POINT ( 'NONE',  ( -16.87231408860552051, -20.68405295654727993, -231.0270656955280515 ) ) ;
#18493 = CARTESIAN_POINT ( 'NONE',  ( -31.04415783139704388, 5.868882651865275690, -221.1472518903637194 ) ) ;
#18494 = CARTESIAN_POINT ( 'NONE',  ( 10.10435529162921853, -13.32996982371095918, -231.5224098423250894 ) ) ;
#18495 = CARTESIAN_POINT ( 'NONE',  ( 22.47485217157460724, -0.5904823501021798648, -216.4383471256914220 ) ) ;
#18496 = CARTESIAN_POINT ( 'NONE',  ( -15.46216926290318305, -2.495270579625169738, -221.2150947962298631 ) ) ;
#18497 = CARTESIAN_POINT ( 'NONE',  ( 19.70286159681817750, 17.87637900817293612, -218.6154571368943493 ) ) ;
#18498 = DIRECTION ( 'NONE',  ( 1.000000000000000000, 0.000000000000000000, 0.000000000000000000 ) ) ;
#18499 = CARTESIAN_POINT ( 'NONE',  ( -12.89119823113977503, 10.10140484475961564, -218.5945808114896636 ) ) ;
#18500 = CARTESIAN_POINT ( 'NONE',  ( 16.73391517716289911, 11.95167056011791828, -233.0268722588312755 ) ) ;
#18501 = VECTOR ( 'NONE', #14017, 1000.000000000000000 ) ;
#18502 = CARTESIAN_POINT ( 'NONE',  ( 16.84848658399567611, 11.39632653812981644, -217.9589513831453473 ) ) ;
#18503 = CARTESIAN_POINT ( 'NONE',  ( 6.295505112925526170, 15.36201163567862693, -221.5772643759389098 ) ) ;
#18504 = CARTESIAN_POINT ( 'NONE',  ( 18.17041142304332624, -16.27896884253082987, -234.9734867155044356 ) ) ;
#18505 = CARTESIAN_POINT ( 'NONE',  ( -8.316505849089994129, 18.84563905716333210, -217.0138378867507640 ) ) ;
#18506 = CARTESIAN_POINT ( 'NONE',  ( -21.08008464085897060, -0.9048411197481797119, -217.0000000010748522 ) ) ;
#18507 = DIRECTION ( 'NONE',  ( 0.000000000000000000, 0.000000000000000000, -1.000000000000000000 ) ) ;
#18508 = CARTESIAN_POINT ( 'NONE',  ( 17.43816562714825125, 15.15720016074785903, -232.3748236813696906 ) ) ;
#18509 = CARTESIAN_POINT ( 'NONE',  ( 7.470327549107519616, -12.61959153319410909, -223.5186783388273568 ) ) ;
#18510 = CARTESIAN_POINT ( 'NONE',  ( -15.82622499106666325, 9.895986579907866343, -218.5115209877527604 ) ) ;
#18511 = CARTESIAN_POINT ( 'NONE',  ( -4.715783688792956063, 28.29821729825949816, -228.0423900005874600 ) ) ;
#18512 = CARTESIAN_POINT ( 'NONE',  ( -14.78079095050690661, -5.416970230978240153, -229.7193632018645246 ) ) ;
#18513 = CARTESIAN_POINT ( 'NONE',  ( 17.57135037026572277, 0.09191994211922807634, -232.8447871904542410 ) ) ;
#18515 = CARTESIAN_POINT ( 'NONE',  ( 9.818699534354031755, 13.69084898312510390, -233.4870046949650089 ) ) ;
#18514 = TOROIDAL_SURFACE ( 'NONE', #6296, 9.000000000000001776, 1.000000000000000000 ) ;
#18516 = CARTESIAN_POINT ( 'NONE',  ( 4.340445191644851874, 29.86837761166362881, -227.4879512554873315 ) ) ;
#18517 = CARTESIAN_POINT ( 'NONE',  ( 22.90686649137879627, -15.60507238429272192, -227.8443525802422585 ) ) ;
#18518 = STYLED_ITEM ( 'NONE', ( #10101 ), #21175 ) ;
#18519 = CARTESIAN_POINT ( 'NONE',  ( -23.45299820629349696, -8.666215563591268989, 5.031560091074801733 ) ) ;
#18520 = CARTESIAN_POINT ( 'NONE',  ( 0.000000000000000000, 0.000000000000000000, -105.0000000000000000 ) ) ;
#18521 = CARTESIAN_POINT ( 'NONE',  ( 4.484811161826725900, 15.38298568785217313, -219.4617573400562662 ) ) ;
#18522 = CARTESIAN_POINT ( 'NONE',  ( -14.25383187134801588, -24.74900029534085633, -216.9920501705437630 ) ) ;
#18523 = CARTESIAN_POINT ( 'NONE',  ( 7.958080982411646076, -16.12895853103474408, -217.0903302464454612 ) ) ;
#18524 = CARTESIAN_POINT ( 'NONE',  ( 11.32394539683753720, -15.63383003174572572, -233.0723040138117881 ) ) ;
#18525 = CARTESIAN_POINT ( 'NONE',  ( -8.548213857283494477, 12.07277636836182211, -222.5354997492170241 ) ) ;
#18526 = CARTESIAN_POINT ( 'NONE',  ( 12.00334754111224100, 12.62951371569041115, -228.5814949098771649 ) ) ;
#18527 = CARTESIAN_POINT ( 'NONE',  ( 0.000000000000000000, 23.00000000000000000, 69.99999999999998579 ) ) ;
#18528 = CARTESIAN_POINT ( 'NONE',  ( -16.36835685385702988, 8.002698209344293545, -233.7585018083067894 ) ) ;
#18529 = CARTESIAN_POINT ( 'NONE',  ( -20.35224420216377439, -13.00389602580315085, -219.1266045330881980 ) ) ;
#18530 = CARTESIAN_POINT ( 'NONE',  ( -9.661739055621840322, 20.41227307912577871, -232.0920144483423257 ) ) ;
#18531 = CARTESIAN_POINT ( 'NONE',  ( 26.59731715018858011, 13.56210517473685329, -229.5787264587298466 ) ) ;
#18532 = CARTESIAN_POINT ( 'NONE',  ( -6.388048297418547961, 21.92257289597608150, -233.3290245341164848 ) ) ;
#18533 = CARTESIAN_POINT ( 'NONE',  ( 24.68599888815047194, -16.20242508705913309, -228.6174911781957633 ) ) ;
#18534 = CARTESIAN_POINT ( 'NONE',  ( 0.000000000000000000, 0.000000000000000000, -55.00000000000000711 ) ) ;
#18535 = CIRCLE ( 'NONE', #20993, 3.000000000000002665 ) ;
#18536 = ORIENTED_EDGE ( 'NONE', *, *, #4685, .T. ) ;
#18537 = CIRCLE ( 'NONE', #19941, 20.99999999999999645 ) ;
#18538 = CARTESIAN_POINT ( 'NONE',  ( -18.47334320050258327, 24.79293862780133040, -226.9986786077537317 ) ) ;
#18539 = CARTESIAN_POINT ( 'NONE',  ( -20.48546531633906298, -12.23885716989380157, -214.8851912114337210 ) ) ;
#18540 = CARTESIAN_POINT ( 'NONE',  ( 0.000000000000000000, 0.000000000000000000, 75.00000000000000000 ) ) ;
#18541 = CARTESIAN_POINT ( 'NONE',  ( 7.769483725421269860, 20.68783433326350263, -233.2348178266662728 ) ) ;
#18542 = CARTESIAN_POINT ( 'NONE',  ( 0.000000000000000000, 0.000000000000000000, -120.0000000000000142 ) ) ;
#18543 = CARTESIAN_POINT ( 'NONE',  ( 22.14671607713456325, -14.13547298543019437, -218.1897693226341914 ) ) ;
#18544 = SURFACE_STYLE_USAGE ( .BOTH. , #15397 ) ;
#18545 = CARTESIAN_POINT ( 'NONE',  ( -17.88126539071149779, 5.766250685202066961, -232.9050303536861293 ) ) ;
#18546 = EDGE_CURVE ( 'NONE', #9212, #16736, #6194, .T. ) ;
#18547 = CARTESIAN_POINT ( 'NONE',  ( -24.33894786102607455, 16.69464852328507831, -227.6320542475859554 ) ) ;
#18548 = CARTESIAN_POINT ( 'NONE',  ( 18.84307465506600465, 4.899879697440840509, -218.2189947030338715 ) ) ;
#18549 = CARTESIAN_POINT ( 'NONE',  ( -5.218961787268129093, -16.18493974670746027, -219.8229902141834771 ) ) ;
#18550 = DIRECTION ( 'NONE',  ( 1.000000000000000000, 0.000000000000000000, 0.000000000000000000 ) ) ;
#18551 = CARTESIAN_POINT ( 'NONE',  ( 14.22574309452842733, 4.476723532073429546, -225.5862451792618231 ) ) ;
#18552 = CARTESIAN_POINT ( 'NONE',  ( -23.00000000000000000, 0.000000000000000000, -60.00000000000000000 ) ) ;
#18553 = CARTESIAN_POINT ( 'NONE',  ( 21.83031488338151149, -1.542591969257156803, -231.3901500139511427 ) ) ;
#18554 = CIRCLE ( 'NONE', #5610, 23.00000000000008882 ) ;
#18555 = CARTESIAN_POINT ( 'NONE',  ( -16.21268175593173311, -5.852138355245464219, -231.1837890105803410 ) ) ;
#18556 = CARTESIAN_POINT ( 'NONE',  ( 0.000000000000000000, -17.50000000000000711, -55.00000000000000000 ) ) ;
#18557 = DIRECTION ( 'NONE',  ( 0.000000000000000000, -1.000000000000000000, 0.000000000000000000 ) ) ;
#18558 = CARTESIAN_POINT ( 'NONE',  ( 5.365126951644291431, 19.60085171667039816, -218.9155869426879519 ) ) ;
#18559 = CARTESIAN_POINT ( 'NONE',  ( 9.097608097968041818, -8.678217757318975600, -221.4288273931462641 ) ) ;
#18560 = CARTESIAN_POINT ( 'NONE',  ( 21.53087031351596892, -21.03550532031109555, -227.1077645633325233 ) ) ;
#18561 = ORIENTED_EDGE ( 'NONE', *, *, #273, .T. ) ;
#18562 = CARTESIAN_POINT ( 'NONE',  ( -12.67219131930435694, 19.52425521811199971, -218.0046184995277372 ) ) ;
#18563 = CARTESIAN_POINT ( 'NONE',  ( -18.46822229429615447, 3.027586163204024405, -230.1002726880134333 ) ) ;
#18564 = CARTESIAN_POINT ( 'NONE',  ( 18.14488609917747652, 6.993670804558928644, -231.4804853770579882 ) ) ;
#18565 = CARTESIAN_POINT ( 'NONE',  ( -13.27091111731893847, -21.09541201825366841, -219.8810390191036106 ) ) ;
#18566 = CARTESIAN_POINT ( 'NONE',  ( 7.548384491377941430, -7.680646770330602280, 91.99999999999998579 ) ) ;
#18567 = CARTESIAN_POINT ( 'NONE',  ( -14.63872435137796302, 9.306825831109410530, -216.0000338566471214 ) ) ;
#18568 = ORIENTED_EDGE ( 'NONE', *, *, #70, .F. ) ;
#18569 = CARTESIAN_POINT ( 'NONE',  ( 11.41911493375616260, 8.796695304819765582, -229.7440655656592412 ) ) ;
#18570 = CARTESIAN_POINT ( 'NONE',  ( 10.59565547865383728, -13.75865772189005476, -221.5384683668846435 ) ) ;
#18571 = CARTESIAN_POINT ( 'NONE',  ( 4.301648988406530094, 13.23079486486395240, -223.2766268961034655 ) ) ;
#18572 = CARTESIAN_POINT ( 'NONE',  ( -11.46843428684449151, 6.508406145394057596, -225.7212143570321814 ) ) ;
#18573 = AXIS2_PLACEMENT_3D ( 'NONE', #6418, #22175, #14988 ) ;
#18574 = EDGE_CURVE ( 'NONE', #17512, #9712, #12736, .T. ) ;
#18575 = CARTESIAN_POINT ( 'NONE',  ( 10.93653298376230687, 10.42959444671468106, -232.5920418140667039 ) ) ;
#18576 = CARTESIAN_POINT ( 'NONE',  ( -24.05551141223569545, 2.266836731622281498, -230.7594878221277384 ) ) ;
#18577 = CARTESIAN_POINT ( 'NONE',  ( -12.74846050492543625, 19.93509882904884734, -216.0172840992881049 ) ) ;
#18578 = CARTESIAN_POINT ( 'NONE',  ( 7.871778267153376696, 7.352373015921426891, 92.00000000000000000 ) ) ;
#18579 = CARTESIAN_POINT ( 'NONE',  ( 6.136979247480394584, 21.37054498543370684, -230.9985475420231467 ) ) ;
#18580 = DIRECTION ( 'NONE',  ( 0.000000000000000000, 0.000000000000000000, -1.000000000000000000 ) ) ;
#18581 = CARTESIAN_POINT ( 'NONE',  ( 0.000000000000000000, 0.000000000000000000, -60.00000000000000000 ) ) ;
#18582 = DIRECTION ( 'NONE',  ( -1.000000000000000000, 0.000000000000000000, 0.000000000000000000 ) ) ;
#18583 = CARTESIAN_POINT ( 'NONE',  ( -16.81617677814535128, 0.6259372974186930838, -233.5115673467681745 ) ) ;
#18584 = CARTESIAN_POINT ( 'NONE',  ( -14.02540557227298024, -18.71004003062420651, -218.0769645724313932 ) ) ;
#18585 = CARTESIAN_POINT ( 'NONE',  ( 18.76166303929370827, 3.000000000000011990, -225.1219455178571707 ) ) ;
#18586 = CARTESIAN_POINT ( 'NONE',  ( -11.85645341316062051, 18.51497629668490674, -217.8828067666886454 ) ) ;
#18587 = CARTESIAN_POINT ( 'NONE',  ( 2.179383121900682951, -16.00498718933496889, -221.0566978482307832 ) ) ;
#18588 = CARTESIAN_POINT ( 'NONE',  ( 22.22999428328319382, 14.15012104770485557, -232.1858878619060249 ) ) ;
#18589 = CARTESIAN_POINT ( 'NONE',  ( -4.784012432433236484, 23.31984772163034947, -232.0554186943449508 ) ) ;
#18590 = CARTESIAN_POINT ( 'NONE',  ( -21.64120863631820413, 17.87363223393748868, -233.1390268986752119 ) ) ;
#18591 = ORIENTED_EDGE ( 'NONE', *, *, #20425, .T. ) ;
#18592 = CARTESIAN_POINT ( 'NONE',  ( -23.72332483825893235, -1.495203899552344007, -219.0564715008207770 ) ) ;
#18593 = CARTESIAN_POINT ( 'NONE',  ( 13.61707622192329481, 14.84143455326118932, -217.6958999636067063 ) ) ;
#18594 = CARTESIAN_POINT ( 'NONE',  ( -15.12838653695630420, 3.161599240781852949, -225.7834014684609656 ) ) ;
#18595 = CARTESIAN_POINT ( 'NONE',  ( -27.56397725925346975, 4.259055856374357241, -222.4951663284069241 ) ) ;
#18596 = DIRECTION ( 'NONE',  ( -1.000000000000000000, 0.000000000000000000, 0.000000000000000000 ) ) ;
#18597 = CARTESIAN_POINT ( 'NONE',  ( -30.62445638522240188, 0.2907099072661952222, -224.9999970559163387 ) ) ;
#18598 = CARTESIAN_POINT ( 'NONE',  ( 6.566035546683759883, 15.06745272174450712, -218.8330720708048034 ) ) ;
#18599 = CARTESIAN_POINT ( 'NONE',  ( -14.67397018911906770, 9.031553917454052893, -228.4349422195089119 ) ) ;
#18600 = CARTESIAN_POINT ( 'NONE',  ( 2.469769522101480597, 18.85781121334172639, -215.5372409425634430 ) ) ;
#18601 = CARTESIAN_POINT ( 'NONE',  ( 19.87150736056128864, 8.436445599727830924, -233.0166429845654932 ) ) ;
#18602 = EDGE_CURVE ( 'NONE', #20426, #14639, #3668, .T. ) ;
#18603 = ORIENTED_EDGE ( 'NONE', *, *, #21825, .T. ) ;
#18604 = CARTESIAN_POINT ( 'NONE',  ( -10.60443131906876246, -11.12562719024938396, -217.6076818590567257 ) ) ;
#18605 = EDGE_LOOP ( 'NONE', ( #6669, #15416, #7612, #4592 ) ) ;
#18606 = CARTESIAN_POINT ( 'NONE',  ( -15.95714424191699266, -19.90201571590360885, -231.7641511196865451 ) ) ;
#18607 = CARTESIAN_POINT ( 'NONE',  ( -30.66857674073067130, 4.440060741118782239, -229.9901150862898476 ) ) ;
#18608 = CARTESIAN_POINT ( 'NONE',  ( 5.569356713096689226, -12.06902110579006226, -223.1407905962607003 ) ) ;
#18609 = CARTESIAN_POINT ( 'NONE',  ( 15.24707275637840453, -5.950922448839978784, -232.7034617680506869 ) ) ;
#18610 = CARTESIAN_POINT ( 'NONE',  ( -22.51170993270524789, -14.32174306031543054, -231.7292175355062795 ) ) ;
#18611 = CARTESIAN_POINT ( 'NONE',  ( 13.60311248493089131, 7.003372205918751092, -219.1738832909067867 ) ) ;
#18612 = CARTESIAN_POINT ( 'NONE',  ( -22.56777165119825668, 2.763754931652832307E-15, 90.00000000000000000 ) ) ;
#18613 = CARTESIAN_POINT ( 'NONE',  ( -14.83806045519817829, 13.18806197935771074, -233.4179411789645542 ) ) ;
#18614 = CARTESIAN_POINT ( 'NONE',  ( 24.49559427486850893, 14.86117239466233642, -230.3058416388274736 ) ) ;
#18615 = CARTESIAN_POINT ( 'NONE',  ( 12.53674998645855787, 17.96979015029927851, -232.8843215672231679 ) ) ;
#18616 = CARTESIAN_POINT ( 'NONE',  ( 12.83388873239664996, 22.07510045760132655, -230.4740059944613222 ) ) ;
#18617 = CARTESIAN_POINT ( 'NONE',  ( 23.13778136609039038, -14.60301800679963335, -216.4810713267295341 ) ) ;
#18618 = CARTESIAN_POINT ( 'NONE',  ( -4.021035526861677312, 25.02763064454595110, -216.6167103172201678 ) ) ;
#18619 = CARTESIAN_POINT ( 'NONE',  ( -15.15110768032078070, 3.517015312212880218, -219.5479300368539270 ) ) ;
#18620 = CARTESIAN_POINT ( 'NONE',  ( -6.938893903907228378E-15, 0.000000000000000000, -224.9999999999999716 ) ) ;
#18621 = CARTESIAN_POINT ( 'NONE',  ( 0.000000000000000000, 0.000000000000000000, -77.51594804401857175 ) ) ;
#18622 = CARTESIAN_POINT ( 'NONE',  ( 3.737366178615106893, -15.16223317163647621, -230.3303395318446292 ) ) ;
#18623 = CARTESIAN_POINT ( 'NONE',  ( -12.33203608746942237, 8.428128317385924717, -222.9277009507565026 ) ) ;
#18624 = CARTESIAN_POINT ( 'NONE',  ( 7.772443558932104146, 25.24620711463332157, -231.7813173736589931 ) ) ;
#18625 = CARTESIAN_POINT ( 'NONE',  ( -12.44777057840899559, -8.577008958641105352, -229.4809580173677830 ) ) ;
#18626 = CARTESIAN_POINT ( 'NONE',  ( 20.10109416526603709, 2.018147939476731434, -216.1034161917718848 ) ) ;
#18627 = CARTESIAN_POINT ( 'NONE',  ( 9.533850545951205291, 16.09136358716069637, -215.9093469876620475 ) ) ;
#18628 = VERTEX_POINT ( 'NONE', #19689 ) ;
#18629 = CARTESIAN_POINT ( 'NONE',  ( 5.141746912158045468, 22.01688500372448232, -216.6678693612369386 ) ) ;
#18630 = CARTESIAN_POINT ( 'NONE',  ( 14.72885890443278889, -12.34426796497947620, -219.7005447341389868 ) ) ;
#18631 = CARTESIAN_POINT ( 'NONE',  ( 17.56598174185312899, -13.96259959359126768, -216.8519506175684626 ) ) ;
#18632 = DIRECTION ( 'NONE',  ( -6.123233995736766036E-17, 0.000000000000000000, 1.000000000000000000 ) ) ;
#18633 = CARTESIAN_POINT ( 'NONE',  ( 7.769483725421269860, 20.68783433326350263, -233.2348178266662728 ) ) ;
#18634 = CARTESIAN_POINT ( 'NONE',  ( -28.63642022368215478, -8.327690832987633129, -230.6787490302224057 ) ) ;
#18635 = CARTESIAN_POINT ( 'NONE',  ( -6.722478243781921492, -14.20656108661463612, -231.4169491518476889 ) ) ;
#18636 = CARTESIAN_POINT ( 'NONE',  ( 14.65870393774896030, -26.09170264574407838, -221.2973805112574723 ) ) ;
#18637 = CARTESIAN_POINT ( 'NONE',  ( -10.76972226383489506, 9.682563335906554158, -229.2555443445334333 ) ) ;
#18638 = CARTESIAN_POINT ( 'NONE',  ( 10.32480721127626033, 15.84468581819879773, -230.0799086455579072 ) ) ;
#18639 = CARTESIAN_POINT ( 'NONE',  ( -16.63766460830045091, 5.158675778507696208, -232.1659425527909093 ) ) ;
#18640 = CARTESIAN_POINT ( 'NONE',  ( -19.01002492504315811, 19.85266905124972681, -219.0021410556803687 ) ) ;
#18641 = CARTESIAN_POINT ( 'NONE',  ( -14.27379873579015879, -4.865929470441826332, -223.9216412988620561 ) ) ;
#18642 = VERTEX_POINT ( 'NONE', #15097 ) ;
#18643 = CARTESIAN_POINT ( 'NONE',  ( -7.375127652145912371, 13.01042140126078195, -223.9959097520547004 ) ) ;
#18644 = CARTESIAN_POINT ( 'NONE',  ( 11.64932556965463561, 7.668732705389711413, -229.0406978839571366 ) ) ;
#18645 = CARTESIAN_POINT ( 'NONE',  ( 8.463901354249619757, 8.457277735286822917, -222.5555366599873821 ) ) ;
#18646 = ADVANCED_FACE ( 'NONE', ( #6867 ), #8337, .T. ) ;
#18647 = CIRCLE ( 'NONE', #12527, 2.000000000000000000 ) ;
#18648 = CARTESIAN_POINT ( 'NONE',  ( 28.96372477351199137, -10.18960100487436904, -225.5971803650229504 ) ) ;
#18649 = CARTESIAN_POINT ( 'NONE',  ( -23.00000000000000000, 0.000000000000000000, 69.99999999999998579 ) ) ;
#18650 = VERTEX_POINT ( 'NONE', #6524 ) ;
#18651 = CARTESIAN_POINT ( 'NONE',  ( -26.74045434827795020, 12.41518252455047744, -220.4617428697642652 ) ) ;
#18652 = CARTESIAN_POINT ( 'NONE',  ( -11.54310632260721903, -10.65784888458977697, -232.4489430773787149 ) ) ;
#18653 = DIRECTION ( 'NONE',  ( 0.000000000000000000, 0.000000000000000000, 1.000000000000000000 ) ) ;
#18654 = CARTESIAN_POINT ( 'NONE',  ( 18.29617186523616468, 23.20920553663278341, -223.4372550713720216 ) ) ;
#18655 = DIRECTION ( 'NONE',  ( -0.000000000000000000, 0.000000000000000000, -1.000000000000000000 ) ) ;
#18656 = CARTESIAN_POINT ( 'NONE',  ( 25.69672030403964769, -15.30292110028031338, -224.0206579222720791 ) ) ;
#18657 =( LENGTH_UNIT ( ) NAMED_UNIT ( * ) SI_UNIT ( .MILLI., .METRE. ) );
#18658 = CARTESIAN_POINT ( 'NONE',  ( -25.61997837663875188, 10.01664178086244483, -231.6711741719404074 ) ) ;
#18659 = CARTESIAN_POINT ( 'NONE',  ( -8.005900519654911562, 11.01772743098285545, -228.7074549843708269 ) ) ;
#18660 = CARTESIAN_POINT ( 'NONE',  ( 18.78616100366561881, 3.045752412654093355, -231.5393376370170699 ) ) ;
#18661 = CARTESIAN_POINT ( 'NONE',  ( -2.389036117848273300, -16.12222041688038132, -229.2542492100865559 ) ) ;
#18662 = CARTESIAN_POINT ( 'NONE',  ( 0.000000000000000000, 0.000000000000000000, 77.51594804401857175 ) ) ;
#18663 = CARTESIAN_POINT ( 'NONE',  ( 21.13193872423781627, -0.8515989525826406226, -222.1182130314809910 ) ) ;
#18664 = CARTESIAN_POINT ( 'NONE',  ( 0.000000000000000000, 0.000000000000000000, -75.00000000000000000 ) ) ;
#18665 = CARTESIAN_POINT ( 'NONE',  ( 12.71657619101469194, -13.18628128886902040, -219.4305778833985414 ) ) ;
#18666 = CARTESIAN_POINT ( 'NONE',  ( 12.85638490943064660, -2.799177453791098280, -223.9042890815753424 ) ) ;
#18667 = CARTESIAN_POINT ( 'NONE',  ( 21.56733749965853164, -0.4285765077750153251, -227.9704549226337917 ) ) ;
#18668 = CARTESIAN_POINT ( 'NONE',  ( 8.162622027327667951, 13.88735946031204094, -224.7165241036068153 ) ) ;
#18669 = CARTESIAN_POINT ( 'NONE',  ( 16.03771109128167538, -13.01076189404929195, -214.9179096003404084 ) ) ;
#18670 = CARTESIAN_POINT ( 'NONE',  ( 15.65513449100897780, -26.00057195821942457, -227.4103383097017570 ) ) ;
#18671 = ORIENTED_EDGE ( 'NONE', *, *, #20887, .T. ) ;
#18672 = CARTESIAN_POINT ( 'NONE',  ( -10.16319438574952372, 11.71174522937666040, -227.8434026503654479 ) ) ;
#18673 = CARTESIAN_POINT ( 'NONE',  ( 17.66525298603349370, 4.919957226727790456, -233.3736646485340032 ) ) ;
#18674 = CARTESIAN_POINT ( 'NONE',  ( 13.17424634425744046, 10.51488364724239588, -221.4616598107521099 ) ) ;
#18675 = ORIENTED_EDGE ( 'NONE', *, *, #9202, .F. ) ;
#18676 = CARTESIAN_POINT ( 'NONE',  ( -3.542274070161974375, -15.57207032904040389, -222.0010230139451437 ) ) ;
#18677 = CARTESIAN_POINT ( 'NONE',  ( -14.20274344593240734, 3.344898002356411659, 93.00000000000000000 ) ) ;
#18678 = CARTESIAN_POINT ( 'NONE',  ( -16.99821283087967672, -0.5135051709387361552, -216.2173766440975555 ) ) ;
#18679 = CARTESIAN_POINT ( 'NONE',  ( 12.58577552758108986, 11.40439409249366420, -217.4478085440898951 ) ) ;
#18680 = CARTESIAN_POINT ( 'NONE',  ( 9.923626285694149729, -13.24753681723166210, -222.8613851586638361 ) ) ;
#18681 = CARTESIAN_POINT ( 'NONE',  ( 1.773982976645536835, 19.12448993322812285, -233.2315972735944172 ) ) ;
#18682 = CARTESIAN_POINT ( 'NONE',  ( -17.79285498209129202, 9.187865686019035749, -216.3798185811636756 ) ) ;
#18683 = CARTESIAN_POINT ( 'NONE',  ( 10.02118533929671074, 10.65166262057242008, -217.7534731326719566 ) ) ;
#18684 = CARTESIAN_POINT ( 'NONE',  ( -21.01482965301294925, 6.368220028842532798, -231.7530032521518990 ) ) ;
#18685 = CARTESIAN_POINT ( 'NONE',  ( -1.881996891245037995, 28.05344686410985489, -218.6379207300106202 ) ) ;
#18686 = DIRECTION ( 'NONE',  ( -0.9940043559354229119, 0.1093404791529896669, -4.060016141862974029E-14 ) ) ;
#18687 = CARTESIAN_POINT ( 'NONE',  ( 6.166782020495575445, -26.61202787628535660, -217.6604608484729795 ) ) ;
#18688 = CARTESIAN_POINT ( 'NONE',  ( 15.13105790938820228, -1.902449014147146178, -222.1588331224812407 ) ) ;
#18689 = DIRECTION ( 'NONE',  ( -1.000000000000000000, -0.000000000000000000, -0.000000000000000000 ) ) ;
#18690 = DIRECTION ( 'NONE',  ( 1.000000000000000000, 0.000000000000000000, 0.000000000000000000 ) ) ;
#18691 = CARTESIAN_POINT ( 'NONE',  ( -17.22166590524039265, 4.587137274468266135, -215.4863060638890033 ) ) ;
#18692 = CARTESIAN_POINT ( 'NONE',  ( -10.96310611394154755, -12.59072721579616605, -220.6792497830813318 ) ) ;
#18693 = DIRECTION ( 'NONE',  ( -0.000000000000000000, -0.000000000000000000, 1.000000000000000000 ) ) ;
#18694 = SURFACE_STYLE_USAGE ( .BOTH. , #13745 ) ;
#18695 = CARTESIAN_POINT ( 'NONE',  ( 5.719431426348611680, -15.09047950350996281, -220.7788505835459318 ) ) ;
#18696 = CARTESIAN_POINT ( 'NONE',  ( 11.35656094503625901, 14.01405796444069018, -230.6944611846958537 ) ) ;
#18697 = CARTESIAN_POINT ( 'NONE',  ( -11.48592899399814726, 13.65854631785387774, -230.8311022452805616 ) ) ;
#18698 = CARTESIAN_POINT ( 'NONE',  ( -21.50655177804914686, 20.61731362457859973, -218.7935603611527426 ) ) ;
#18699 = VERTEX_POINT ( 'NONE', #5054 ) ;
#18700 = CARTESIAN_POINT ( 'NONE',  ( 31.90367160121947876, -0.9372977198352894224, -223.6547426844143445 ) ) ;
#18701 = ORIENTED_EDGE ( 'NONE', *, *, #12124, .F. ) ;
#18702 = CARTESIAN_POINT ( 'NONE',  ( 9.586902571418640662, 24.43292817174309661, -231.9968623198229807 ) ) ;
#18703 = CARTESIAN_POINT ( 'NONE',  ( -26.70018640714903668, 3.110792036746048428, -228.8761207540193823 ) ) ;
#18704 = CARTESIAN_POINT ( 'NONE',  ( -21.89065952084834166, -0.9940043559354216907, -218.9999999999999716 ) ) ;
#18705 = DIRECTION ( 'NONE',  ( 0.000000000000000000, 0.000000000000000000, -1.000000000000000000 ) ) ;
#18706 = CARTESIAN_POINT ( 'NONE',  ( 11.63337745479824292, 8.229076005436313679, -220.5472098800687206 ) ) ;
#18707 = CARTESIAN_POINT ( 'NONE',  ( -17.55809605150417951, 6.636094600389130349, -229.8856864643722986 ) ) ;
#18708 = CARTESIAN_POINT ( 'NONE',  ( 6.812728368504421539, 14.35307019806973194, -216.7766581591129977 ) ) ;
#18709 = CARTESIAN_POINT ( 'NONE',  ( 24.60354977307301283, 7.993510024274534942, -218.5358880819990759 ) ) ;
#18710 = CARTESIAN_POINT ( 'NONE',  ( -3.294080042861979862, -13.96442541267666826, -227.2909938985368683 ) ) ;
#18711 = ORIENTED_EDGE ( 'NONE', *, *, #7214, .T. ) ;
#18712 = CARTESIAN_POINT ( 'NONE',  ( -10.95598939193837928, -18.74794674280272488, -217.4432683290776538 ) ) ;
#18713 = CARTESIAN_POINT ( 'NONE',  ( -14.63872435137796302, 9.306825831109410530, -216.0000338566471214 ) ) ;
#18714 = CARTESIAN_POINT ( 'NONE',  ( 5.451525948382545117, -12.45300865616632713, -227.8545162512558306 ) ) ;
#18715 = CARTESIAN_POINT ( 'NONE',  ( -7.825349071214003693, 24.14595706726266755, -216.5959661901539732 ) ) ;
#18716 = CARTESIAN_POINT ( 'NONE',  ( 9.867031390707305505, -6.965612358230354850, -226.9368589251366188 ) ) ;
#18717 = CARTESIAN_POINT ( 'NONE',  ( -18.75993824683981970, -9.028840681436806292, -217.1556094966459227 ) ) ;
#18718 = CARTESIAN_POINT ( 'NONE',  ( 26.72610819325501907, 14.97064052581051108, -224.6384473985499426 ) ) ;
#18719 = LINE ( 'NONE', #10168, #22112 ) ;
#18720 = CARTESIAN_POINT ( 'NONE',  ( -21.72273972318264867, 21.08396222359856864, -224.0477214759881690 ) ) ;
#18721 = CARTESIAN_POINT ( 'NONE',  ( 11.75069299018312208, 6.043853022588032253, -224.2604610870103841 ) ) ;
#18722 = CARTESIAN_POINT ( 'NONE',  ( 12.58590500897257947, 11.38573988265384607, -230.4867078522624695 ) ) ;
#18723 = CARTESIAN_POINT ( 'NONE',  ( 8.179023008129211902, 20.84698146175953681, -218.6376653143925921 ) ) ;
#18724 = CARTESIAN_POINT ( 'NONE',  ( -3.600307272616782406, -16.89541809348436630, -217.5924753110707570 ) ) ;
#18725 = CARTESIAN_POINT ( 'NONE',  ( -4.651113456395510326, 27.58151660986499110, -218.3072938287727141 ) ) ;
#18726 = CARTESIAN_POINT ( 'NONE',  ( 13.54927135793711557, 0.6749664302445949060, -222.0769159577524192 ) ) ;
#18727 = CARTESIAN_POINT ( 'NONE',  ( 4.072690587420734865, -13.44063513242216246, -222.4530508649998239 ) ) ;
#18728 = CARTESIAN_POINT ( 'NONE',  ( -16.07193224038526580, 12.24477688577882439, -232.1409653212175499 ) ) ;
#18729 = CARTESIAN_POINT ( 'NONE',  ( 0.1556102272723409452, 19.71550568250159685, -232.1993058477363547 ) ) ;
#18730 = CARTESIAN_POINT ( 'NONE',  ( -18.64257584594551531, -16.66392856591270899, -217.1407738418131999 ) ) ;
#18731 = CARTESIAN_POINT ( 'NONE',  ( 17.66525298603349370, 4.919957226727790456, -233.3736646485340032 ) ) ;
#18732 = CARTESIAN_POINT ( 'NONE',  ( 19.20222574149634909, 21.83532798770326266, -218.6913543321078919 ) ) ;
#18733 = EDGE_LOOP ( 'NONE', ( #12273, #11912, #14243, #2025, #14544, #1487 ) ) ;
#18734 = CARTESIAN_POINT ( 'NONE',  ( -3.501680520304516264, 14.31538576447642264, -219.8967178229432307 ) ) ;
#18735 = CARTESIAN_POINT ( 'NONE',  ( 14.50342097185254353, -4.720444175079822280, -222.5922120714632513 ) ) ;
#18736 = CARTESIAN_POINT ( 'NONE',  ( 19.75516891782859474, -3.344025276999063934, -216.3638920815759263 ) ) ;
#18737 = DIRECTION ( 'NONE',  ( -0.000000000000000000, 0.000000000000000000, -1.000000000000000000 ) ) ;
#18738 = CARTESIAN_POINT ( 'NONE',  ( -3.843007962268670585, 27.94983497691806917, -231.4302614368887703 ) ) ;
#18739 = CARTESIAN_POINT ( 'NONE',  ( -24.74482344071061135, -7.641957171360318490, -233.9284114646162891 ) ) ;
#18740 = CARTESIAN_POINT ( 'NONE',  ( -7.349743644505656093, -15.31718010764164539, -232.4470764718129772 ) ) ;
#18741 = CARTESIAN_POINT ( 'NONE',  ( 16.07085865561684201, -17.65509622858733252, -216.6880805489183501 ) ) ;
#18742 = CARTESIAN_POINT ( 'NONE',  ( -9.115411286166651195, 13.66191091052436235, -230.3338332872444312 ) ) ;
#18743 = CARTESIAN_POINT ( 'NONE',  ( 16.48099188159542194, 16.04875567542346815, -230.8408106201084706 ) ) ;
#18744 = CARTESIAN_POINT ( 'NONE',  ( -25.80904414196669450, 12.19501778665756220, -219.1732313092283846 ) ) ;
#18745 = CARTESIAN_POINT ( 'NONE',  ( -25.00745438246740804, 14.90779342625281778, -219.2410538611701156 ) ) ;
#18746 = CARTESIAN_POINT ( 'NONE',  ( -12.38412712796990434, -11.70129718676926878, -221.8135637406489025 ) ) ;
#18747 = CARTESIAN_POINT ( 'NONE',  ( -7.464187997994982560, 14.20693289415472016, -228.8865298551900764 ) ) ;
#18748 = CARTESIAN_POINT ( 'NONE',  ( 13.20340559785743828, 9.575208899273587093, -218.1210831379648312 ) ) ;
#18749 = CARTESIAN_POINT ( 'NONE',  ( 6.550054208186137039, 12.38618022562281595, -231.5087189857719068 ) ) ;
#18750 = CARTESIAN_POINT ( 'NONE',  ( 20.28526114930425450, -5.837089636085359245, -233.7994602772149051 ) ) ;
#18751 = LINE ( 'NONE', #1313, #12169 ) ;
#18752 = ORIENTED_EDGE ( 'NONE', *, *, #16821, .F. ) ;
#18753 = ADVANCED_FACE ( 'NONE', ( #3250 ), #12685, .T. ) ;
#18754 = CARTESIAN_POINT ( 'NONE',  ( -3.843007962268670585, 27.94983497691806917, -231.4302614368887703 ) ) ;
#18755 = CARTESIAN_POINT ( 'NONE',  ( -23.71722460534674681, -17.39027245378339259, -231.9193655574418074 ) ) ;
#18756 = DIRECTION ( 'NONE',  ( -0.000000000000000000, -0.000000000000000000, -1.000000000000000000 ) ) ;
#18757 = CIRCLE ( 'NONE', #12998, 17.50000000000007816 ) ;
#18758 = CARTESIAN_POINT ( 'NONE',  ( 14.54149994592679107, 8.070685273005897997, -229.7292930672863349 ) ) ;
#18759 = CARTESIAN_POINT ( 'NONE',  ( 21.53087031351596892, -21.03550532031109555, -227.1077645633325233 ) ) ;
#18760 = CARTESIAN_POINT ( 'NONE',  ( -12.78558550453068854, 7.693178343823584342, -230.0800953344970878 ) ) ;
#18761 = PRODUCT ( 'BR-822', 'BR-822', '', ( #7832 ) ) ;
#18762 = CARTESIAN_POINT ( 'NONE',  ( 18.55287065739596031, 7.869864349944380777, -232.8430408253643691 ) ) ;
#18763 = CARTESIAN_POINT ( 'NONE',  ( -5.429593058350183910, -25.95961553913046416, -230.5291520159703111 ) ) ;
#18764 = AXIS2_PLACEMENT_3D ( 'NONE', #6010, #12666, #21304 ) ;
#18765 = FACE_OUTER_BOUND ( 'NONE', #21123, .T. ) ;
#18766 = ADVANCED_FACE ( 'NONE', ( #20125, #3142 ), #15208, .F. ) ;
#18767 = CARTESIAN_POINT ( 'NONE',  ( 20.28602808787868739, -1.649471991126303827, -222.4662206817569370 ) ) ;
#18768 = CARTESIAN_POINT ( 'NONE',  ( 0.000000000000000000, 0.000000000000000000, 77.51594804401857175 ) ) ;
#18769 = CARTESIAN_POINT ( 'NONE',  ( 11.44298997664856721, -19.26084286805135193, -217.6324489131326914 ) ) ;
#18770 = CARTESIAN_POINT ( 'NONE',  ( 1.232595164407830946E-29, -17.50000000000007105, -30.00000000000000000 ) ) ;
#18771 = CARTESIAN_POINT ( 'NONE',  ( 20.12875910279704073, -1.792218354162612881, -227.4130037078831776 ) ) ;
#18772 = CARTESIAN_POINT ( 'NONE',  ( 12.84032013659066251, 19.10303921738740485, -230.8110334357214128 ) ) ;
#18773 = CIRCLE ( 'NONE', #13755, 3.000000000000002665 ) ;
#18774 = CARTESIAN_POINT ( 'NONE',  ( 11.16964468591631920, 25.71443501674299981, -224.7497461878887464 ) ) ;
#18775 = ADVANCED_FACE ( 'NONE', ( #11709 ), #6872, .F. ) ;
#18776 = CARTESIAN_POINT ( 'NONE',  ( 12.00030915192824565, -12.23229153226815313, -233.8665814532129730 ) ) ;
#18777 = CARTESIAN_POINT ( 'NONE',  ( 13.96958060839473958, -9.488587112651741151, -218.7731372952745232 ) ) ;
#18778 = APPLICATION_CONTEXT ( 'automotive_design' ) ;
#18779 = CARTESIAN_POINT ( 'NONE',  ( -8.407534899841293097, 16.91942258446019665, -231.3029992963236339 ) ) ;
#18780 = CARTESIAN_POINT ( 'NONE',  ( -14.20363567091065349, 7.857660128015216294, -223.4151327167956822 ) ) ;
#18781 = CARTESIAN_POINT ( 'NONE',  ( 17.24423567610276109, 8.542587572837451404, -218.6562240232607621 ) ) ;
#18782 = ORIENTED_EDGE ( 'NONE', *, *, #9403, .T. ) ;
#18783 = CARTESIAN_POINT ( 'NONE',  ( -2.076897692258683925, -29.27639190819841275, -225.1343076284445601 ) ) ;
#18784 = CARTESIAN_POINT ( 'NONE',  ( -7.647666590413455090, -7.580942749559344662, 92.00000000000000000 ) ) ;
#18785 = VERTEX_POINT ( 'NONE', #11594 ) ;
#18786 = CARTESIAN_POINT ( 'NONE',  ( 16.77055746703809191, 7.081497542956901370, -232.0295235404293521 ) ) ;
#18787 = CARTESIAN_POINT ( 'NONE',  ( 17.47473467751515486, -18.15791173363047051, -230.0427332633545632 ) ) ;
#18788 = CARTESIAN_POINT ( 'NONE',  ( 2.008896548638861024, 20.64812324442097591, -233.5818019448501843 ) ) ;
#18789 = CARTESIAN_POINT ( 'NONE',  ( -18.08305592660031991, 4.022743421239192152, -217.2335041149100050 ) ) ;
#18790 = CIRCLE ( 'NONE', #19138, 2.000000000000000000 ) ;
#18791 = CIRCLE ( 'NONE', #22000, 21.63401512838748175 ) ;
#18792 = CARTESIAN_POINT ( 'NONE',  ( 6.812728368504421539, 14.35307019806973194, -216.7766581591129977 ) ) ;
#18793 = CARTESIAN_POINT ( 'NONE',  ( -24.53276002501160136, 17.12571705644413811, -226.2419685911331442 ) ) ;
#18794 = CARTESIAN_POINT ( 'NONE',  ( 0.2389779871941385414, 16.64595486589868045, -218.1658233406367629 ) ) ;
#18795 = LINE ( 'NONE', #10245, #11279 ) ;
#18796 = CARTESIAN_POINT ( 'NONE',  ( -2.576162127940193169, -15.57202066281789321, -231.6911579627040396 ) ) ;
#18797 = CARTESIAN_POINT ( 'NONE',  ( 27.36047156164216787, -8.591464759722228450, -221.3690063136810977 ) ) ;
#18798 = DIRECTION ( 'NONE',  ( -1.000000000000000000, 0.000000000000000000, 0.000000000000000000 ) ) ;
#18799 = CARTESIAN_POINT ( 'NONE',  ( -15.57331739480619248, 4.297375044201914740, -216.4079605712025511 ) ) ;
#18800 = CARTESIAN_POINT ( 'NONE',  ( -20.83288780491947279, -19.75659621676223665, -225.4831129403879117 ) ) ;
#18801 = AXIS2_PLACEMENT_3D ( 'NONE', #16793, #9931, #6429 ) ;
#18802 = CARTESIAN_POINT ( 'NONE',  ( 4.999282783285113219, -13.99249059192112021, -223.3817383379047214 ) ) ;
#18803 = CARTESIAN_POINT ( 'NONE',  ( -18.88895772509644644, 1.306698388790553444, -217.6272550812279292 ) ) ;
#18804 = CARTESIAN_POINT ( 'NONE',  ( 3.080453011304693511, 29.32691491905673331, -222.8956499783474499 ) ) ;
#18805 = CARTESIAN_POINT ( 'NONE',  ( -8.523771322135640816, 24.09653697920728987, -233.1071395647740303 ) ) ;
#18806 = ORIENTED_EDGE ( 'NONE', *, *, #7092, .T. ) ;
#18807 = CARTESIAN_POINT ( 'NONE',  ( 13.85225051576513700, -1.547701942753643145, -218.6451083988944788 ) ) ;
#18808 = CARTESIAN_POINT ( 'NONE',  ( 12.18657022793382794, 26.76558097653315471, -221.8882195427397335 ) ) ;
#18809 = CARTESIAN_POINT ( 'NONE',  ( -15.82952867276381603, 3.677461268355039170, -227.9997968350711801 ) ) ;
#18810 = CARTESIAN_POINT ( 'NONE',  ( -13.66744685701839046, 5.938820276054873837, -223.0954633396572149 ) ) ;
#18811 = CARTESIAN_POINT ( 'NONE',  ( -13.53581065110708970, -26.13331550560631555, -224.9773145811678887 ) ) ;
#18812 = LINE ( 'NONE', #3383, #6206 ) ;
#18813 = CARTESIAN_POINT ( 'NONE',  ( 10.95881707662767290, 12.06788758096456782, -231.4359029166177208 ) ) ;
#18814 = AXIS2_PLACEMENT_3D ( 'NONE', #17596, #2163, #9043 ) ;
#18815 = CARTESIAN_POINT ( 'NONE',  ( -23.99493126334580850, 6.052326449358573335, -219.7958990219547672 ) ) ;
#18816 = CARTESIAN_POINT ( 'NONE',  ( 1.867752180833619713, 31.25122076096762669, -227.4007918511463231 ) ) ;
#18817 = CARTESIAN_POINT ( 'NONE',  ( 26.53121369294028042, 10.74560293343441586, -229.2288136770759195 ) ) ;
#18818 = CARTESIAN_POINT ( 'NONE',  ( -12.16163208632051784, -17.84934472108236747, -234.2417547270719638 ) ) ;
#18819 = ORIENTED_EDGE ( 'NONE', *, *, #8587, .F. ) ;
#18820 = CARTESIAN_POINT ( 'NONE',  ( -11.57846532275044460, -10.37575015818511304, -229.3776965522603462 ) ) ;
#18821 = CARTESIAN_POINT ( 'NONE',  ( -14.12265793148702464, 24.49085167151569919, -218.3312790639385241 ) ) ;
#18822 = CARTESIAN_POINT ( 'NONE',  ( 1.729916699924999746, -18.64927252049523432, -233.5000329212076906 ) ) ;
#18823 = CARTESIAN_POINT ( 'NONE',  ( 0.7245137624042983227, 13.44764381486384330, -223.4043886706536455 ) ) ;
#18824 = CARTESIAN_POINT ( 'NONE',  ( 9.734612854996214537, -6.789898087979761243, -225.0934417779699004 ) ) ;
#18825 = CARTESIAN_POINT ( 'NONE',  ( -15.19144047750087267, -10.24270553329939304, -232.4311702607364793 ) ) ;
#18826 = CARTESIAN_POINT ( 'NONE',  ( 22.16968511661519869, 1.542591969257184337, -234.6098499860488573 ) ) ;
#18827 = CARTESIAN_POINT ( 'NONE',  ( -24.63401512838748530, 3.016796777712720900E-15, -77.51594804401857175 ) ) ;
#18828 = CARTESIAN_POINT ( 'NONE',  ( -5.125319492185865577, 20.53749879880200524, -218.7557759432853288 ) ) ;
#18829 = CARTESIAN_POINT ( 'NONE',  ( 9.931717191100288389, 12.93133689537362940, -228.8926047089119038 ) ) ;
#18830 = CARTESIAN_POINT ( 'NONE',  ( 13.61707622192329481, 14.84143455326118932, -217.6958999636067063 ) ) ;
#18831 = CARTESIAN_POINT ( 'NONE',  ( 17.34461553379066601, 6.893916422670210764, -233.3442385185644525 ) ) ;
#18832 = CARTESIAN_POINT ( 'NONE',  ( -0.1378336831626507664, -14.33879523207274964, -230.9095596798049144 ) ) ;
#18833 = AXIS2_PLACEMENT_3D ( 'NONE', #15059, #7967, #2879 ) ;
#18834 = CARTESIAN_POINT ( 'NONE',  ( -9.969679877803788060, 12.84542071557917176, -220.4758784541224657 ) ) ;
#18835 = CARTESIAN_POINT ( 'NONE',  ( 18.60971343765040942, 2.368090295052050820, -218.6871071987073094 ) ) ;
#18836 = CARTESIAN_POINT ( 'NONE',  ( 10.12607331509846986, -17.07097861414113638, -217.9029769802564545 ) ) ;
#18837 = CARTESIAN_POINT ( 'NONE',  ( -17.39737143130126285, 7.531548707695031375, -232.0788227848755696 ) ) ;
#18838 = CARTESIAN_POINT ( 'NONE',  ( 8.674175678922351196, 20.85307874897338110, -216.6688793998777101 ) ) ;
#18839 = ADVANCED_FACE ( 'NONE', ( #22172 ), #13630, .T. ) ;
#18840 = CARTESIAN_POINT ( 'NONE',  ( -28.18501077041064562, -8.523171531337160545, -227.0531053546762337 ) ) ;
#18841 = CARTESIAN_POINT ( 'NONE',  ( 25.50289296650958448, 5.998088869914441901, -233.1161630295026157 ) ) ;
#18842 = CARTESIAN_POINT ( 'NONE',  ( 20.02669998934234741, 11.93441252203826508, -216.7824909737982182 ) ) ;
#18843 = CARTESIAN_POINT ( 'NONE',  ( 18.29617186523616468, 23.20920553663278341, -223.4372550713720216 ) ) ;
#18844 = CARTESIAN_POINT ( 'NONE',  ( 22.40610909459028122, -16.32493987272327018, -222.3848458449739951 ) ) ;
#18845 = CARTESIAN_POINT ( 'NONE',  ( 13.09169075717699293, -6.869491136113572871, -220.8313809912125691 ) ) ;
#18846 = CIRCLE ( 'NONE', #17076, 3.000000000000002665 ) ;
#18847 = CARTESIAN_POINT ( 'NONE',  ( 10.07175337281514871, 14.76776740066196325, -231.7834566702614723 ) ) ;
#18848 = CARTESIAN_POINT ( 'NONE',  ( -26.65136949509196640, -16.37772123076025466, -229.1931346627563073 ) ) ;
#18849 = CARTESIAN_POINT ( 'NONE',  ( -14.24095617957673632, -25.86326826095433162, -229.7068514753157160 ) ) ;
#18850 = CARTESIAN_POINT ( 'NONE',  ( 12.84024077373997841, -14.50125846907313054, -216.8496453050001946 ) ) ;
#18851 = CARTESIAN_POINT ( 'NONE',  ( -21.29946384424354733, 21.01772963953914442, -222.5871995662667757 ) ) ;
#18852 = CARTESIAN_POINT ( 'NONE',  ( 8.647507700742417924, 16.42978512283924175, -220.3082116258600536 ) ) ;
#18853 = CARTESIAN_POINT ( 'NONE',  ( -13.93333636822611155, 3.327141996558931947, -221.4468162587888287 ) ) ;
#18854 = CARTESIAN_POINT ( 'NONE',  ( -6.407569900110946293, 14.82357759665407215, -221.6203916094852957 ) ) ;
#18855 = CARTESIAN_POINT ( 'NONE',  ( -24.12156516248416693, -2.505154625461648799, -217.3585533157102248 ) ) ;
#18856 = VERTEX_POINT ( 'NONE', #3030 ) ;
#18857 = CARTESIAN_POINT ( 'NONE',  ( -17.14223598032838325, 23.31797360549976261, -226.5771676936548431 ) ) ;
#18858 = CARTESIAN_POINT ( 'NONE',  ( 18.23116248274160256, 13.99874872632082123, -216.0593560670294835 ) ) ;
#18859 = CARTESIAN_POINT ( 'NONE',  ( 25.17176037151762813, 18.95054595444721102, -221.3490360113488862 ) ) ;
#18860 = CARTESIAN_POINT ( 'NONE',  ( 18.79106389458910442, -5.302521403133691358, -233.5021979784848440 ) ) ;
#18861 = DIRECTION ( 'NONE',  ( 0.000000000000000000, 0.000000000000000000, -1.000000000000000000 ) ) ;
#18862 = ORIENTED_EDGE ( 'NONE', *, *, #14770, .T. ) ;
#18863 = CARTESIAN_POINT ( 'NONE',  ( -2.208416658185406334, 29.10348627872611615, -219.8480645685746424 ) ) ;
#18864 = CARTESIAN_POINT ( 'NONE',  ( -16.01199461824852932, -9.140529685459805265, -215.3147469429904106 ) ) ;
#18865 = CARTESIAN_POINT ( 'NONE',  ( -24.63401512838757768, 0.000000000000000000, 77.51594804401857175 ) ) ;
#18866 = AXIS2_PLACEMENT_3D ( 'NONE', #12542, #16888, #10135 ) ;
#18867 = CARTESIAN_POINT ( 'NONE',  ( 24.57222455393806015, 12.08236629421828212, -229.7319216558644541 ) ) ;
#18868 = CARTESIAN_POINT ( 'NONE',  ( -14.29986196492902550, 0.06805469746732484282, -227.4167624117703213 ) ) ;
#18869 = CARTESIAN_POINT ( 'NONE',  ( 23.44296991241933981, -12.51566675729016964, -231.4065378011870564 ) ) ;
#18870 = CARTESIAN_POINT ( 'NONE',  ( -15.48255455842386219, 10.01793346089237069, -233.1197357361336913 ) ) ;
#18871 = ADVANCED_FACE ( 'NONE', ( #9917 ), #12668, .T. ) ;
#18872 = CARTESIAN_POINT ( 'NONE',  ( -13.93333636822611155, 3.327141996558931947, -221.4468162587888287 ) ) ;
#18873 = CARTESIAN_POINT ( 'NONE',  ( 1.268102448827562068, -18.18084990330622830, -231.0699201170278911 ) ) ;
#18874 = DIRECTION ( 'NONE',  ( -1.000000000000000000, 0.000000000000000000, 0.000000000000000000 ) ) ;
#18875 = CARTESIAN_POINT ( 'NONE',  ( 0.000000000000000000, 0.000000000000000000, -30.00000000000000000 ) ) ;
#18876 = DIRECTION ( 'NONE',  ( 0.000000000000000000, 0.000000000000000000, -1.000000000000000000 ) ) ;
#18877 = CARTESIAN_POINT ( 'NONE',  ( 10.54788747927062964, -11.30141756528536412, -223.8337882627521651 ) ) ;
#18879 = EDGE_CURVE ( 'NONE', #14742, #8296, #6526, .T. ) ;
#18878 = CARTESIAN_POINT ( 'NONE',  ( 12.81768984168529357, -2.998094226192216549, -225.2178905539254004 ) ) ;
#18880 = DIRECTION ( 'NONE',  ( 1.000000000000000000, 0.000000000000000000, 0.000000000000000000 ) ) ;
#18881 = CARTESIAN_POINT ( 'NONE',  ( 5.112468059216026539, 15.05346046978967856, -223.6558835435016590 ) ) ;
#18882 = CARTESIAN_POINT ( 'NONE',  ( 0.7903203334012884884, 21.30772501796948859, -217.9064416298261619 ) ) ;
#18883 = CARTESIAN_POINT ( 'NONE',  ( 9.478576170506354259, -9.424747406754709900, -230.1309108789951949 ) ) ;
#18884 = CIRCLE ( 'NONE', #20287, 2.000000000000000000 ) ;
#18885 = CARTESIAN_POINT ( 'NONE',  ( 17.28140336138120858, -11.48510652344925020, -216.9852223368602893 ) ) ;
#18886 = VERTEX_POINT ( 'NONE', #16890 ) ;
#18887 = AXIS2_PLACEMENT_3D ( 'NONE', #21854, #7817, #940 ) ;
#18888 = CARTESIAN_POINT ( 'NONE',  ( -10.70754874174748039, 23.84972878377777405, -230.7991598016655246 ) ) ;
#18889 = CARTESIAN_POINT ( 'NONE',  ( -17.00819119081011266, 8.904695857470725784, -219.7915043529501133 ) ) ;
#18890 = CARTESIAN_POINT ( 'NONE',  ( -16.36835685385702988, 8.002698209344293545, -233.7585018083067894 ) ) ;
#18891 = CARTESIAN_POINT ( 'NONE',  ( -14.04270955969662360, -23.25437626513260980, -222.0989702864435174 ) ) ;
#18892 = CARTESIAN_POINT ( 'NONE',  ( 1.455845656607146809E-13, -21.63401512838747820, -77.51594804401857175 ) ) ;
#18893 = ORIENTED_EDGE ( 'NONE', *, *, #9134, .F. ) ;
#18894 = CARTESIAN_POINT ( 'NONE',  ( 14.21126657910812874, 6.833562750302326627, -220.2783117037562874 ) ) ;
#18895 = CARTESIAN_POINT ( 'NONE',  ( 15.57652300565637482, -15.79620443381692496, -231.0117242343698081 ) ) ;
#18896 = EDGE_CURVE ( 'NONE', #10628, #497, #8364, .T. ) ;
#18897 = CARTESIAN_POINT ( 'NONE',  ( 7.168644370073567806, 19.32044210858112265, -233.1278450877711634 ) ) ;
#18898 = CARTESIAN_POINT ( 'NONE',  ( -14.83974801774860630, 13.71714848582103485, -216.0935642439352762 ) ) ;
#18899 = CARTESIAN_POINT ( 'NONE',  ( 16.22460398937575121, -0.7285105026664867589, -219.3274985887512116 ) ) ;
#18900 = CARTESIAN_POINT ( 'NONE',  ( -18.39892766464214446, 25.11039525536027739, -225.3444503920457294 ) ) ;
#18901 = CARTESIAN_POINT ( 'NONE',  ( -22.10934047915427314, 0.9940043559354312386, -216.9999999999999716 ) ) ;
#18902 = CARTESIAN_POINT ( 'NONE',  ( 1.780803752597676537, -13.83832444325970101, -229.2250779460899537 ) ) ;
#18903 = CARTESIAN_POINT ( 'NONE',  ( 19.06763123184207487, -2.048228142369658666, -218.2337357994572073 ) ) ;
#18904 = CYLINDRICAL_SURFACE ( 'NONE', #5579, 23.00000000000008882 ) ;
#18905 = CARTESIAN_POINT ( 'NONE',  ( -19.31342342724724759, -3.870051895940637365, -217.8584481481169348 ) ) ;
#18906 = CARTESIAN_POINT ( 'NONE',  ( -17.58289524052909414, 0.7988212499981205417, -233.9567931471624149 ) ) ;
#18907 = CARTESIAN_POINT ( 'NONE',  ( -13.44952714103469305, -17.53057434768947331, -217.9956016333683237 ) ) ;
#18908 = CARTESIAN_POINT ( 'NONE',  ( 4.823266655078461085, -13.86048651889774241, -224.7145696108100026 ) ) ;
#18909 = CARTESIAN_POINT ( 'NONE',  ( -28.61025869263052712, 6.891613135096296361, -222.2489362813765013 ) ) ;
#18910 = CARTESIAN_POINT ( 'NONE',  ( 0.8374361358884788720, 23.73768315274483953, -232.4065959030912154 ) ) ;
#18911 = CARTESIAN_POINT ( 'NONE',  ( -7.903959818038710061, 11.02445096303677552, -229.5951168968472871 ) ) ;
#18912 = EDGE_LOOP ( 'NONE', ( #17874, #3801, #18208, #17102, #13542, #15143 ) ) ;
#18913 = CARTESIAN_POINT ( 'NONE',  ( 30.30402220111207612, -9.997565949388443229, -221.8870099070453250 ) ) ;
#18914 = EDGE_LOOP ( 'NONE', ( #11778, #8413, #12428, #19654, #17458 ) ) ;
#18915 = PRESENTATION_LAYER_ASSIGNMENT (  '', '', ( #20325 ) ) ;
#18916 = CARTESIAN_POINT ( 'NONE',  ( 12.53674998645855787, 17.96979015029927851, -232.8843215672231679 ) ) ;
#18917 = CARTESIAN_POINT ( 'NONE',  ( -14.30586181932858914, 18.69563132175512266, -215.8217153853723573 ) ) ;
#18918 = CARTESIAN_POINT ( 'NONE',  ( -22.18165477997343871, 9.502253276305026475, -218.0070055737419636 ) ) ;
#18919 = CARTESIAN_POINT ( 'NONE',  ( -11.24961133108761935, -10.18645864713539950, -228.7780882195199013 ) ) ;
#18920 = ADVANCED_FACE ( 'NONE', ( #5056 ), #6550, .T. ) ;
#18921 = CARTESIAN_POINT ( 'NONE',  ( -17.50000000000000711, 0.000000000000000000, -30.00000000000000000 ) ) ;
#18922 = CARTESIAN_POINT ( 'NONE',  ( 21.77183241683778547, 12.04504704525620085, -233.6005549158834640 ) ) ;
#18923 = CARTESIAN_POINT ( 'NONE',  ( -16.45414350258782221, 17.57852913985137988, -231.3969631806205598 ) ) ;
#18924 = CARTESIAN_POINT ( 'NONE',  ( 21.77779027533950540, 18.43917590911969029, -232.9503911151153659 ) ) ;
#18925 = CARTESIAN_POINT ( 'NONE',  ( 24.81668481317358399, 17.11438712655213124, -222.1096362285750274 ) ) ;
#18926 = CARTESIAN_POINT ( 'NONE',  ( -25.31373219958254595, -16.11658482301340811, -218.6250613297025609 ) ) ;
#18927 = ORIENTED_EDGE ( 'NONE', *, *, #3252, .F. ) ;
#18928 = CARTESIAN_POINT ( 'NONE',  ( -8.652743106909156268, -19.89692808811530966, -232.3032230114403376 ) ) ;
#18929 = CARTESIAN_POINT ( 'NONE',  ( -7.686214453470440411, 10.71593237010305444, -228.8058998235944159 ) ) ;
#18930 = CARTESIAN_POINT ( 'NONE',  ( 13.36656406724190305, -19.73987914515934960, -233.3798509643240209 ) ) ;
#18931 = CARTESIAN_POINT ( 'NONE',  ( -2.934221234790329369, 15.07857928364152222, -230.9558365497803720 ) ) ;
#18932 = CARTESIAN_POINT ( 'NONE',  ( 10.88145840916109819, -7.482884786208209960, -219.8679920012262414 ) ) ;
#18933 = CARTESIAN_POINT ( 'NONE',  ( -18.89430729770302975, -12.42271633246521212, -233.2230176520695295 ) ) ;
#18934 = CARTESIAN_POINT ( 'NONE',  ( 12.15450584778660570, 2.288537795953278220, -225.7049340319972828 ) ) ;
#18935 = FILL_AREA_STYLE_COLOUR ( '', #17820 ) ;
#18936 = CARTESIAN_POINT ( 'NONE',  ( -8.881241380679488984, 27.18697625135247975, -224.4474391433207927 ) ) ;
#18937 = CARTESIAN_POINT ( 'NONE',  ( -14.58575946311604277, 2.190332613129932327, -228.6717927865686590 ) ) ;
#18938 = CARTESIAN_POINT ( 'NONE',  ( 11.87982377808925527, 10.85265283465803421, -229.5027252913499183 ) ) ;
#18939 = CARTESIAN_POINT ( 'NONE',  ( 10.97349919442152810, 9.416813005082010690, -227.3764328406868742 ) ) ;
#18940 = CARTESIAN_POINT ( 'NONE',  ( 3.979505144402133876, -26.19079129315300491, -216.2323960841296469 ) ) ;
#18941 = CARTESIAN_POINT ( 'NONE',  ( 12.75306435971521068, 14.56583715532477186, -214.9711136650476533 ) ) ;
#18942 = CARTESIAN_POINT ( 'NONE',  ( 15.52719855059926424, 1.633696074270991172, -221.7349885876216433 ) ) ;
#18943 = CARTESIAN_POINT ( 'NONE',  ( -5.856318878364832337, -22.45395696943396402, -215.0711972856051943 ) ) ;
#18944 = CARTESIAN_POINT ( 'NONE',  ( -16.12870690754239078, 23.19263481078822053, -221.6099859194323471 ) ) ;
#18945 = CARTESIAN_POINT ( 'NONE',  ( -4.224287562409271501, 29.03635716824519264, -224.1823526280761882 ) ) ;
#18946 = CARTESIAN_POINT ( 'NONE',  ( -13.05629324012484282, -10.24599397043673221, -218.7452066004821347 ) ) ;
#18947 = CARTESIAN_POINT ( 'NONE',  ( -22.19349712985372491, 11.03542788991621748, -219.7744882786627443 ) ) ;
#18948 = CARTESIAN_POINT ( 'NONE',  ( 11.20580770355584299, 27.81589616365139150, -231.3138133330081132 ) ) ;
#18949 = ORIENTED_EDGE ( 'NONE', *, *, #16032, .F. ) ;
#18950 = CARTESIAN_POINT ( 'NONE',  ( 16.54345861550681107, 19.37554510112122230, -218.2240151908141002 ) ) ;
#18951 = CARTESIAN_POINT ( 'NONE',  ( 21.29805123434030634, -10.14609140759417905, -218.4136040999194108 ) ) ;
#18952 = ORIENTED_EDGE ( 'NONE', *, *, #4317, .F. ) ;
#18953 = CARTESIAN_POINT ( 'NONE',  ( 17.93010821528303822, -10.80507700282924688, -233.3968735006674251 ) ) ;
#18954 = SURFACE_SIDE_STYLE ('',( #282 ) ) ;
#18955 = CARTESIAN_POINT ( 'NONE',  ( 16.84848658399567611, 11.39632653812981644, -217.9589513831453473 ) ) ;
#18956 = CARTESIAN_POINT ( 'NONE',  ( -24.71505016400469756, -15.67489082254766508, -232.1683526798342143 ) ) ;
#18957 = CARTESIAN_POINT ( 'NONE',  ( 0.5120693878963755719, -30.63998626839889639, -227.9504769009175220 ) ) ;
#18958 = CARTESIAN_POINT ( 'NONE',  ( 11.14834367153813233, -21.42845646353120870, -216.4520112529555718 ) ) ;
#18959 = CARTESIAN_POINT ( 'NONE',  ( 1.820119372073704112, 23.17972341190215246, -230.7270437017659503 ) ) ;
#18960 = LINE ( 'NONE', #8095, #6569 ) ;
#18961 = CARTESIAN_POINT ( 'NONE',  ( 15.70179827786738969, 6.572001003133339125, -229.5476218741844434 ) ) ;
#18962 = CARTESIAN_POINT ( 'NONE',  ( -27.29953305526601426, 11.21644211419729054, -229.3676346105362995 ) ) ;
#18963 = CARTESIAN_POINT ( 'NONE',  ( -11.88513743913613752, 17.65694776598872195, -232.6054623148957035 ) ) ;
#18964 = CARTESIAN_POINT ( 'NONE',  ( 28.96372477351199137, -10.18960100487436904, -225.5971803650229504 ) ) ;
#18965 = CARTESIAN_POINT ( 'NONE',  ( 2.579827969572558111, 15.91317371615649101, -219.7652087782269916 ) ) ;
#18966 = EDGE_CURVE ( 'NONE', #9583, #14565, #18791, .T. ) ;
#18967 = CARTESIAN_POINT ( 'NONE',  ( -21.99356461413155728, 5.827088221545293045, -219.1725956997024127 ) ) ;
#18968 = CARTESIAN_POINT ( 'NONE',  ( 12.58033168766476528, 20.35631482982274676, -235.1670639654690547 ) ) ;
#18969 = CARTESIAN_POINT ( 'NONE',  ( 10.44758276073090109, -14.65753298717242714, -218.5965683461722904 ) ) ;
#18970 = ORIENTED_EDGE ( 'NONE', *, *, #3485, .F. ) ;
#18971 = CARTESIAN_POINT ( 'NONE',  ( -8.966714183099560032, 19.05224306381768073, -234.0879867025980445 ) ) ;
#18972 = CARTESIAN_POINT ( 'NONE',  ( -10.60443131906876246, -11.12562719024938396, -217.6076818590567257 ) ) ;
#18973 = DIRECTION ( 'NONE',  ( 0.000000000000000000, 0.000000000000000000, -1.000000000000000000 ) ) ;
#18974 = CARTESIAN_POINT ( 'NONE',  ( 15.76910524310159900, 5.601482066865847820, -220.3440822020379528 ) ) ;
#18975 = CARTESIAN_POINT ( 'NONE',  ( -27.82842955277035202, 11.70195273568964112, -227.9294339757464911 ) ) ;
#18976 = CARTESIAN_POINT ( 'NONE',  ( 19.06212547406409641, -9.287000003594721775, -232.7453815625877667 ) ) ;
#18977 = SURFACE_STYLE_FILL_AREA ( #12461 ) ;
#18978 = CARTESIAN_POINT ( 'NONE',  ( -15.20262116893801974, 8.038155052917188570, -217.6767387945475036 ) ) ;
#18979 = CARTESIAN_POINT ( 'NONE',  ( -14.29986196492902550, 0.06805469746732484282, -227.4167624117703213 ) ) ;
#18980 = CARTESIAN_POINT ( 'NONE',  ( -4.650330424930598561, -23.85841421069521928, -231.7493909980149454 ) ) ;
#18981 = CARTESIAN_POINT ( 'NONE',  ( 10.76794919243112325, 1.424750975061700904E-15, 95.00000000000000000 ) ) ;
#18982 = CARTESIAN_POINT ( 'NONE',  ( 15.53193985890930406, 1.024324097469592187, -227.8693888979224198 ) ) ;
#18983 = CARTESIAN_POINT ( 'NONE',  ( -15.82069055112642353, 8.315535108674763976, -217.2800172218543935 ) ) ;
#18984 = CARTESIAN_POINT ( 'NONE',  ( 17.50516624540364319, -11.67908417450482794, -218.9956384138364740 ) ) ;
#18985 = CARTESIAN_POINT ( 'NONE',  ( 14.59755125472582016, -2.008934638541916229, -227.2287433509217465 ) ) ;
#18986 = CARTESIAN_POINT ( 'NONE',  ( -23.13355025916758834, 9.482198088197261399, 3.242749661402037020 ) ) ;
#18987 = CARTESIAN_POINT ( 'NONE',  ( 14.40184562439531213, 6.414772937171507650, -227.4651811604036595 ) ) ;
#18988 = CARTESIAN_POINT ( 'NONE',  ( -7.399925907206128528, 10.29859031525428037, -227.1614041762800298 ) ) ;
#18989 = TOROIDAL_SURFACE ( 'NONE', #13979, 24.63401512838747820, 3.000000000000000888 ) ;
#18990 = CARTESIAN_POINT ( 'NONE',  ( 16.48099188159542194, 16.04875567542346815, -230.8408106201084706 ) ) ;
#18991 = CARTESIAN_POINT ( 'NONE',  ( -5.110696651857618455, -18.61886646437566384, -231.2604145522360000 ) ) ;
#18992 = CARTESIAN_POINT ( 'NONE',  ( 14.51690190576628048, -4.522004643715366257, -218.3468014590714859 ) ) ;
#18993 = CARTESIAN_POINT ( 'NONE',  ( -22.04240660558204823, 19.10355008918698871, -223.9524535985323723 ) ) ;
#18994 = CARTESIAN_POINT ( 'NONE',  ( -17.30580402557236752, 11.30149179219993982, -230.8639894634705172 ) ) ;
#18995 = CARTESIAN_POINT ( 'NONE',  ( -27.40681729237160269, 15.04232492504307572, -225.3323746796125704 ) ) ;
#18996 = ORIENTED_EDGE ( 'NONE', *, *, #3893, .T. ) ;
#18997 = CARTESIAN_POINT ( 'NONE',  ( -8.182256202386261279, -21.48229377488409497, -218.8195705044138606 ) ) ;
#18998 = CARTESIAN_POINT ( 'NONE',  ( 0.000000000000000000, 0.000000000000000000, 75.00000000000000000 ) ) ;
#18999 = ORIENTED_EDGE ( 'NONE', *, *, #8253, .T. ) ;
#19000 = CARTESIAN_POINT ( 'NONE',  ( 27.58248235015124550, 10.80791576765187934, -226.6933256641281389 ) ) ;
#19001 = CARTESIAN_POINT ( 'NONE',  ( 14.72885890443278889, -12.34426796497947620, -219.7005447341389868 ) ) ;
#19002 = CARTESIAN_POINT ( 'NONE',  ( 11.67669251569587985, 24.04736029062789981, -218.5856804285192254 ) ) ;
#19003 = CARTESIAN_POINT ( 'NONE',  ( -11.33137429837660193, 27.25022425932026238, -230.1650924901870212 ) ) ;
#19004 = ADVANCED_FACE ( 'NONE', ( #2019 ), #2936, .F. ) ;
#19005 = AXIS2_PLACEMENT_3D ( 'NONE', #2005, #330, #7198 ) ;
#19006 = CARTESIAN_POINT ( 'NONE',  ( 21.06229272850552547, 3.434461253538921621, -234.1452885155528918 ) ) ;
#19007 = CARTESIAN_POINT ( 'NONE',  ( 10.07175337281514871, 14.76776740066196325, -231.7834566702614723 ) ) ;
#19008 = CARTESIAN_POINT ( 'NONE',  ( -10.55034688490273709, 2.476137110235850258, 92.00000000000001421 ) ) ;
#19009 = CARTESIAN_POINT ( 'NONE',  ( 0.04660897052267574947, -31.13860575300111577, -224.7746869833732717 ) ) ;
#19010 = CARTESIAN_POINT ( 'NONE',  ( 20.38902395782249144, -18.95772103455488633, -230.9098670703349967 ) ) ;
#19011 = CARTESIAN_POINT ( 'NONE',  ( 1.387778780781445676E-13, -19.79999999999999716, 78.50000000000000000 ) ) ;
#19012 = DIRECTION ( 'NONE',  ( 0.000000000000000000, 0.000000000000000000, 1.000000000000000000 ) ) ;
#19013 = CARTESIAN_POINT ( 'NONE',  ( -23.68377094563794572, 13.02263794644603578, -215.9752901280847652 ) ) ;
#19014 = CARTESIAN_POINT ( 'NONE',  ( -24.64494147011371084, -8.645298684267959999, -229.1812397229770113 ) ) ;
#19015 = CARTESIAN_POINT ( 'NONE',  ( -20.45797657813638182, 1.164962349958370336, -217.1306074022350572 ) ) ;
#19016 = CARTESIAN_POINT ( 'NONE',  ( 7.163080459435270164, 24.05253566895842354, -232.4475987112033408 ) ) ;
#19017 = CARTESIAN_POINT ( 'NONE',  ( 2.914696262605396715, 19.49933023975583879, -231.6035545612375017 ) ) ;
#19018 = ORIENTED_EDGE ( 'NONE', *, *, #983, .F. ) ;
#19019 = CARTESIAN_POINT ( 'NONE',  ( -22.78589867900506150, -1.373495078166624861, -218.8339345403132370 ) ) ;
#19020 = CARTESIAN_POINT ( 'NONE',  ( 5.623554730548537606, 15.65270319720736225, -231.3185741195121068 ) ) ;
#19021 = CARTESIAN_POINT ( 'NONE',  ( -15.61959985466312872, 8.133362592386543355, -230.7826037412100106 ) ) ;
#19022 = CARTESIAN_POINT ( 'NONE',  ( -22.14646582578067679, 6.967411055428133437, -231.6932229095398270 ) ) ;
#19023 = CARTESIAN_POINT ( 'NONE',  ( -21.50522087930578152, -16.03150550247721640, -231.4768288373508369 ) ) ;
#19024 = CARTESIAN_POINT ( 'NONE',  ( 15.37450427861381286, -5.898921106289613847E-14, -228.0000000000000853 ) ) ;
#19025 = CARTESIAN_POINT ( 'NONE',  ( -25.00000000000010303, 0.000000000000000000, 75.00000000000000000 ) ) ;
#19026 = DIRECTION ( 'NONE',  ( -1.000000000000000000, 1.224646799147353454E-16, 0.000000000000000000 ) ) ;
#19027 = CARTESIAN_POINT ( 'NONE',  ( 26.28575214971901630, 3.591103948354015696, -217.0994821834097763 ) ) ;
#19028 = CARTESIAN_POINT ( 'NONE',  ( -21.01242583983345469, 16.60754347445175227, -220.8286358486543293 ) ) ;
#19029 = CARTESIAN_POINT ( 'NONE',  ( 8.373295497769937867, 8.203271496719947820, -226.1884629658694053 ) ) ;
#19030 = CARTESIAN_POINT ( 'NONE',  ( -17.96792326766206926, -0.6237852504629022299, -217.9759415197746932 ) ) ;
#19031 = CARTESIAN_POINT ( 'NONE',  ( -11.10256751292636324, -5.696117445562730808, -228.9287437256430451 ) ) ;
#19032 = CARTESIAN_POINT ( 'NONE',  ( -17.04082806826102470, -4.797954729550726327, -217.3726213297937306 ) ) ;
#19033 = ADVANCED_FACE ( 'NONE', ( #17329 ), #15546, .T. ) ;
#19034 = CARTESIAN_POINT ( 'NONE',  ( -5.298027976154672025, 13.43376398981453157, -220.6333279128949982 ) ) ;
#19035 = CARTESIAN_POINT ( 'NONE',  ( -6.722478243781921492, -14.20656108661463612, -231.4169491518476889 ) ) ;
#19036 = CARTESIAN_POINT ( 'NONE',  ( -11.02345917017863464, 29.02019856777526741, -223.9475008740665771 ) ) ;
#19037 = CARTESIAN_POINT ( 'NONE',  ( 23.13778136609039038, -14.60301800679963335, -216.4810713267295341 ) ) ;
#19038 = CARTESIAN_POINT ( 'NONE',  ( 15.14614948138922657, -0.1777235777276532369, -227.9951794835837973 ) ) ;
#19039 = EDGE_CURVE ( 'NONE', #3431, #2867, #8711, .T. ) ;
#19040 = CARTESIAN_POINT ( 'NONE',  ( 30.55431851955342282, 7.682798326916945975, -224.9061577511691610 ) ) ;
#19041 = CARTESIAN_POINT ( 'NONE',  ( 0.000000000000000000, 0.000000000000000000, 77.51594804401857175 ) ) ;
#19042 = CARTESIAN_POINT ( 'NONE',  ( -9.175187729848801155, 26.50888816229029743, -227.9285554593684253 ) ) ;
#19043 = CARTESIAN_POINT ( 'NONE',  ( -15.30864812529618391, 1.596444765892653717, -220.3859421844601627 ) ) ;
#19044 = CARTESIAN_POINT ( 'NONE',  ( 14.80394259695730064, 1.224172658189580432, -225.4564070658925061 ) ) ;
#19045 = CARTESIAN_POINT ( 'NONE',  ( 14.19979467405507556, 6.351366891014061267, -230.8614099669030679 ) ) ;
#19046 = CARTESIAN_POINT ( 'NONE',  ( -2.827720241434194648, -28.87017495157254743, -218.9856045314649577 ) ) ;
#19047 = EDGE_CURVE ( 'NONE', #7303, #22217, #12602, .T. ) ;
#19048 = CARTESIAN_POINT ( 'NONE',  ( 9.986779374595107228, 29.47523823012521049, -229.5287702428778687 ) ) ;
#19049 = CARTESIAN_POINT ( 'NONE',  ( -2.000000000000000000, 2.449293598294706414E-16, -70.00000000000000000 ) ) ;
#19050 = CARTESIAN_POINT ( 'NONE',  ( -2.809719670556939608, -23.45209095268191390, -234.3886352793013543 ) ) ;
#19051 = CARTESIAN_POINT ( 'NONE',  ( -12.67219131930435694, 19.52425521811199971, -218.0046184995277372 ) ) ;
#19052 = CARTESIAN_POINT ( 'NONE',  ( 17.31940731551425827, 24.90170669671083914, -222.9868986272316533 ) ) ;
#19053 = CARTESIAN_POINT ( 'NONE',  ( -25.42089018817326007, -6.263968923056941307, -218.6542964065910439 ) ) ;
#19054 = CARTESIAN_POINT ( 'NONE',  ( -25.36936018126600345, 11.57160208538938306, -224.9662154788713622 ) ) ;
#19055 = CARTESIAN_POINT ( 'NONE',  ( -5.582510911615395699, 27.25430150734737111, -233.3200100877314469 ) ) ;
#19056 = CARTESIAN_POINT ( 'NONE',  ( 22.44730228620155899, 3.608729811217749717, -232.0798239124179645 ) ) ;
#19057 = ORIENTED_EDGE ( 'NONE', *, *, #2080, .F. ) ;
#19058 = CARTESIAN_POINT ( 'NONE',  ( 17.97642781552999836, -18.85565020944788373, -229.3765379620127760 ) ) ;
#19059 = CARTESIAN_POINT ( 'NONE',  ( 5.719431426348611680, -15.09047950350996281, -220.7788505835459318 ) ) ;
#19060 = APPLICATION_CONTEXT ( 'automotive_design' ) ;
#19061 = CARTESIAN_POINT ( 'NONE',  ( -2.543684969149407227, 16.28137730373167713, -227.6987697727321915 ) ) ;
#19062 = CARTESIAN_POINT ( 'NONE',  ( 10.78187269046063435, 10.73871010366167944, -221.9206544238666368 ) ) ;
#19063 = CARTESIAN_POINT ( 'NONE',  ( 27.96460686140487084, -1.872811165202790340, -220.9791906660856000 ) ) ;
#19064 = CARTESIAN_POINT ( 'NONE',  ( -11.28700884291539630, -21.85791790461604478, -233.5354093188319951 ) ) ;
#19065 = CARTESIAN_POINT ( 'NONE',  ( 7.088126259304779353, -19.25156530781288566, -233.7785425911077937 ) ) ;
#19066 = CARTESIAN_POINT ( 'NONE',  ( -6.407569900110946293, 14.82357759665407215, -221.6203916094852957 ) ) ;
#19067 = DIRECTION ( 'NONE',  ( -0.000000000000000000, -0.000000000000000000, -1.000000000000000000 ) ) ;
#19068 = CARTESIAN_POINT ( 'NONE',  ( 26.92457506054779515, 6.538608665672222209, -219.8654465082432807 ) ) ;
#19069 = CARTESIAN_POINT ( 'NONE',  ( -22.17339560624464312, 16.26550580028390769, -232.0582861498566274 ) ) ;
#19070 = CARTESIAN_POINT ( 'NONE',  ( -8.221702953833418093, 11.87876791566348800, -223.9138461338794741 ) ) ;
#19071 = CARTESIAN_POINT ( 'NONE',  ( -1.772400894765090662, 19.49811434610897010, -217.8797837662441168 ) ) ;
#19072 = CARTESIAN_POINT ( 'NONE',  ( -26.04932551096112192, 5.001193774903864409, -228.9498367494266802 ) ) ;
#19073 = CARTESIAN_POINT ( 'NONE',  ( 12.48419387172699579, 6.663456953110941328, -219.2717027540951165 ) ) ;
#19074 = CARTESIAN_POINT ( 'NONE',  ( 8.339826811406878093, -13.81198187275966660, -229.8741491687588621 ) ) ;
#19075 = CARTESIAN_POINT ( 'NONE',  ( 23.03038449397558196, 0.000000000000000000, 75.34729635533385306 ) ) ;
#19076 = VERTEX_POINT ( 'NONE', #3481 ) ;
#19077 = CARTESIAN_POINT ( 'NONE',  ( -5.807479211365208727, 19.77444019604324410, -216.0778658752277863 ) ) ;
#19078 = CARTESIAN_POINT ( 'NONE',  ( 28.08231343014353243, -2.974470402155979354, -225.4253119135968291 ) ) ;
#19079 = DIRECTION ( 'NONE',  ( -1.000000000000000000, 0.000000000000000000, 0.000000000000000000 ) ) ;
#19080 = CARTESIAN_POINT ( 'NONE',  ( 19.72515656911863147, 14.02277373989196541, -218.0718040828188009 ) ) ;
#19081 = CARTESIAN_POINT ( 'NONE',  ( -18.08305592660031991, 4.022743421239192152, -217.2335041149100050 ) ) ;
#19082 = CARTESIAN_POINT ( 'NONE',  ( 14.65870393774896030, -26.09170264574407838, -221.2973805112574723 ) ) ;
#19083 = CARTESIAN_POINT ( 'NONE',  ( 0.000000000000000000, 0.000000000000000000, 0.000000000000000000 ) ) ;
#19084 = CARTESIAN_POINT ( 'NONE',  ( -17.65835845419170624, 22.55329142274348442, -231.2673511165784532 ) ) ;
#19085 = CARTESIAN_POINT ( 'NONE',  ( -13.11494368899652052, 3.355507568391938200, -225.9121440085824304 ) ) ;
#19086 = CARTESIAN_POINT ( 'NONE',  ( -11.82217545354207644, -11.78227988727524966, -219.0934395369134506 ) ) ;
#19087 = CARTESIAN_POINT ( 'NONE',  ( 0.000000000000000000, 0.000000000000000000, 77.51594804401857175 ) ) ;
#19088 = CARTESIAN_POINT ( 'NONE',  ( -22.56563535238560902, 4.458514667912840679, 8.957021455394174936 ) ) ;
#19089 = CARTESIAN_POINT ( 'NONE',  ( -22.17339560624464312, 16.26550580028390769, -232.0582861498566274 ) ) ;
#19090 = CARTESIAN_POINT ( 'NONE',  ( 14.94445598564424493, -12.06760924077967090, -230.4366326412025785 ) ) ;
#19091 = CARTESIAN_POINT ( 'NONE',  ( -23.14980455159086503, 0.3541108476526578785, -217.8785187302087536 ) ) ;
#19092 = CARTESIAN_POINT ( 'NONE',  ( -22.94128848581996039, 9.935662058461005586, -1.312836635664774043 ) ) ;
#19093 = CARTESIAN_POINT ( 'NONE',  ( 12.91676121433235913, 9.519065828383201477, -226.8102878246443765 ) ) ;
#19094 = CARTESIAN_POINT ( 'NONE',  ( -9.491065840222427497, 13.31995980477872266, -232.8537120564120073 ) ) ;
#19095 = DIRECTION ( 'NONE',  ( -1.000000000000000000, 0.000000000000000000, 0.000000000000000000 ) ) ;
#19096 = CARTESIAN_POINT ( 'NONE',  ( 24.52860916307685457, 12.75391509163817361, -221.3604763108436941 ) ) ;
#19097 = CARTESIAN_POINT ( 'NONE',  ( 3.099569060413221333, -25.61866983817578713, -217.9657659276338677 ) ) ;
#19098 = CARTESIAN_POINT ( 'NONE',  ( 21.26068545928058384, -3.181857413669367141, -233.8217025890263585 ) ) ;
#19099 = ORIENTED_EDGE ( 'NONE', *, *, #22019, .T. ) ;
#19100 = CARTESIAN_POINT ( 'NONE',  ( -1.301562195391901877, 16.19210386685474390, -220.0867867038183192 ) ) ;
#19101 = CARTESIAN_POINT ( 'NONE',  ( -19.72392517715239535, 13.50888179936880107, -230.7714862421596251 ) ) ;
#19102 = CARTESIAN_POINT ( 'NONE',  ( -17.17143024911216287, 2.756036084795755681, -233.9491886983466316 ) ) ;
#19103 = CARTESIAN_POINT ( 'NONE',  ( -21.38043581477633026, -15.61850963832630335, -229.1016256230698502 ) ) ;
#19104 = DIRECTION ( 'NONE',  ( -0.000000000000000000, -0.000000000000000000, -1.000000000000000000 ) ) ;
#19105 = VERTEX_POINT ( 'NONE', #1794 ) ;
#19106 = CARTESIAN_POINT ( 'NONE',  ( 15.46952826979347151, 3.173892190046953665, -221.7237849701489552 ) ) ;
#19107 = CARTESIAN_POINT ( 'NONE',  ( 1.152695246012044095, -27.06931983241920747, -220.0193874843003528 ) ) ;
#19108 = CARTESIAN_POINT ( 'NONE',  ( 10.83706092800007781, 10.12544885278926543, -227.1716144446442343 ) ) ;
#19109 = CARTESIAN_POINT ( 'NONE',  ( -11.42613629117093765, 28.09170287990588832, -228.7150250545069241 ) ) ;
#19110 = AXIS2_PLACEMENT_3D ( 'NONE', #11787, #18653, #3214 ) ;
#19111 = CARTESIAN_POINT ( 'NONE',  ( 16.53896178738450828, 2.691624496798088462, -232.5974196329879078 ) ) ;
#19112 = TOROIDAL_SURFACE ( 'NONE', #1143, 22.00000000000000711, 2.999999999999999112 ) ;
#19113 = CARTESIAN_POINT ( 'NONE',  ( 5.343558017910363667, 26.29639771561252459, -218.1010331760174665 ) ) ;
#19114 = DIRECTION ( 'NONE',  ( 0.000000000000000000, 0.000000000000000000, -1.000000000000000000 ) ) ;
#19115 = CARTESIAN_POINT ( 'NONE',  ( -8.258403559667634397, -29.80786866836635696, -223.3983869762195127 ) ) ;
#19116 = CARTESIAN_POINT ( 'NONE',  ( 8.649266908999912573, -10.50942778440553482, -226.4415026780416440 ) ) ;
#19117 = LINE ( 'NONE', #13964, #8111 ) ;
#19118 = CARTESIAN_POINT ( 'NONE',  ( 0.000000000000000000, 0.000000000000000000, 77.51594804401857175 ) ) ;
#19119 = CARTESIAN_POINT ( 'NONE',  ( -20.38637754046084183, 19.95723714148678241, -217.5201383746364172 ) ) ;
#19120 = CARTESIAN_POINT ( 'NONE',  ( -17.95722789764597849, -8.907256384892455969, -219.4045086951509518 ) ) ;
#19121 = CARTESIAN_POINT ( 'NONE',  ( 21.27683256847563698, 4.223177115764435108, -215.2584548172064842 ) ) ;
#19122 = CARTESIAN_POINT ( 'NONE',  ( 7.213476267053916757, 16.78447451494783138, -217.5857052077849687 ) ) ;
#19123 = CARTESIAN_POINT ( 'NONE',  ( 1.430961520682887400, 16.89318350835024063, -220.3256763723340157 ) ) ;
#19124 = EDGE_LOOP ( 'NONE', ( #6325, #20980, #4364, #15311, #16317 ) ) ;
#19125 = CARTESIAN_POINT ( 'NONE',  ( 11.27265965248755819, -10.15440342946296148, -217.7707216267749573 ) ) ;
#19126 = CARTESIAN_POINT ( 'NONE',  ( 14.73698509926073186, 4.443590625350892331, -227.4062002049096236 ) ) ;
#19127 = AXIS2_PLACEMENT_3D ( 'NONE', #21934, #13737, #6413 ) ;
#19128 = CARTESIAN_POINT ( 'NONE',  ( -8.413706464639300719, 10.92140547936800843, -220.6417935981040728 ) ) ;
#19129 = CARTESIAN_POINT ( 'NONE',  ( -15.60078324628501356, 3.527872497691606934, -227.4630248446626695 ) ) ;
#19130 = CARTESIAN_POINT ( 'NONE',  ( -5.534391910549205207, -14.54353160188980709, -228.1022699408985943 ) ) ;
#19131 = CARTESIAN_POINT ( 'NONE',  ( -14.83974801774860630, 13.71714848582103485, -216.0935642439352762 ) ) ;
#19132 = CARTESIAN_POINT ( 'NONE',  ( 0.000000000000000000, 0.000000000000000000, -77.51594804401857175 ) ) ;
#19133 = CARTESIAN_POINT ( 'NONE',  ( 14.99379536286055625, -2.466525803139443695, -223.2806853455627731 ) ) ;
#19134 = CARTESIAN_POINT ( 'NONE',  ( 30.60340911705754863, 5.703403611927857497, -225.1938343315648297 ) ) ;
#19135 = CARTESIAN_POINT ( 'NONE',  ( -22.38528940623734798, 16.50235888036280230, -227.1443357386333162 ) ) ;
#19136 = CARTESIAN_POINT ( 'NONE',  ( 13.70863938672594529, 6.616599615120571265, -232.1343637516268643 ) ) ;
#19137 = CARTESIAN_POINT ( 'NONE',  ( -21.89482327431018760, 1.733733432562314158, -233.1353281693111796 ) ) ;
#19138 = AXIS2_PLACEMENT_3D ( 'NONE', #10066, #8385, #22099 ) ;
#19139 = CARTESIAN_POINT ( 'NONE',  ( -29.11561446909439965, 0.2226424683783513325, -217.8829860219008765 ) ) ;
#19140 = AXIS2_PLACEMENT_3D ( 'NONE', #21575, #6163, #19886 ) ;
#19141 = CARTESIAN_POINT ( 'NONE',  ( -17.66047203424674450, -3.377913611064220056, -232.7782090104293786 ) ) ;
#19142 = CARTESIAN_POINT ( 'NONE',  ( -22.56222084847001597, 18.89892770556097901, -231.8972396388394088 ) ) ;
#19143 = CARTESIAN_POINT ( 'NONE',  ( -13.13432812001650341, -19.42279346457301514, -216.4126494286626610 ) ) ;
#19145 = B_SPLINE_CURVE_WITH_KNOTS ( 'NONE', 3,
 ( #12741, #14876, #16224, #13184, #14658, #8009, #21385, #19586, #14434, #17919, #9476, #6082, #2484, #7793, #21601, #12957, #799, #7679, #19801, #19694, #11270, #18139 ),
 .UNSPECIFIED., .F., .F.,
 ( 4, 2, 2, 2, 2, 2, 2, 2, 2, 2, 4 ),
 ( -1.095445575531557103E-05, 0.0003522495710956626848, 0.0007154535979466409949, 0.001441861651648580159, 0.002168269705350519324, 0.002894677759052458055, 0.003621085812754397219, 0.004347493866456335516, 0.005073901920158274681, 0.005437105947009245564, 0.005800309973860217315 ),
 .UNSPECIFIED. ) ;
#19144 = CARTESIAN_POINT ( 'NONE',  ( 12.53674998645855787, 17.96979015029927851, -232.8843215672231679 ) ) ;
#19146 = CARTESIAN_POINT ( 'NONE',  ( 4.093437342195941575, -12.31737333437662940, -220.6844603446061512 ) ) ;
#19147 = DIRECTION ( 'NONE',  ( -0.000000000000000000, 0.000000000000000000, -1.000000000000000000 ) ) ;
#19148 = ADVANCED_FACE ( 'NONE', ( #10696 ), #7101, .F. ) ;
#19149 = CARTESIAN_POINT ( 'NONE',  ( 15.14859676485869500, 2.119979922547468032, -231.9009926880791284 ) ) ;
#19150 = CARTESIAN_POINT ( 'NONE',  ( -25.00000000000013500, 1.972152263052529514E-28, 0.000000000000000000 ) ) ;
#19151 = CARTESIAN_POINT ( 'NONE',  ( -1.796846813493219619, 26.08418332695505271, -220.7262848173578504 ) ) ;
#19152 = CARTESIAN_POINT ( 'NONE',  ( -27.52457542293397097, 5.447957517019466067, -230.2717933641555135 ) ) ;
#19153 = CARTESIAN_POINT ( 'NONE',  ( 18.06016678184731461, 2.257982981100609354, -218.9983079406065940 ) ) ;
#19154 = CARTESIAN_POINT ( 'NONE',  ( 30.55431851955342282, 7.682798326916945975, -224.9061577511691610 ) ) ;
#19155 = CARTESIAN_POINT ( 'NONE',  ( 4.772350409791505932, -16.13531085440822466, -233.6884202312745344 ) ) ;
#19156 = CARTESIAN_POINT ( 'NONE',  ( 17.60070748514786132, 25.68479983175475567, -229.9331108608050158 ) ) ;
#19157 = VECTOR ( 'NONE', #19598, 1000.000000000000000 ) ;
#19158 = CIRCLE ( 'NONE', #18465, 21.63401512838748175 ) ;
#19159 = DIRECTION ( 'NONE',  ( 1.000000000000000000, 0.000000000000000000, 0.000000000000000000 ) ) ;
#19160 = CARTESIAN_POINT ( 'NONE',  ( -6.646164377397596468, -30.92684034042379437, -222.9942643485979374 ) ) ;
#19161 = CARTESIAN_POINT ( 'NONE',  ( -13.51991436508781597, 16.61129329384914755, -232.1184346153593197 ) ) ;
#19162 = ADVANCED_FACE ( 'NONE', ( #3813 ), #11233, .F. ) ;
#19163 = CARTESIAN_POINT ( 'NONE',  ( 6.491278574642851851, 13.23281603069746382, -229.0355254242266767 ) ) ;
#19164 = CARTESIAN_POINT ( 'NONE',  ( -29.22168435891936156, -1.352755938724206519, -225.9547066689444250 ) ) ;
#19165 = CARTESIAN_POINT ( 'NONE',  ( -17.30580402557236752, 11.30149179219993982, -230.8639894634705172 ) ) ;
#19166 = CARTESIAN_POINT ( 'NONE',  ( -1.302381543002304687, 18.65968181418110206, -215.1730913991678449 ) ) ;
#19167 = CARTESIAN_POINT ( 'NONE',  ( 15.57986488780344736, -0.6155558446892130942, -225.2777919203616932 ) ) ;
#19168 = ORIENTED_EDGE ( 'NONE', *, *, #1211, .F. ) ;
#19169 = CARTESIAN_POINT ( 'NONE',  ( 11.72806877847873253, -14.77654346318461975, -220.1368134445341695 ) ) ;
#19170 = CARTESIAN_POINT ( 'NONE',  ( 18.24334571313621467, -21.83696521683136282, -220.5798317591433886 ) ) ;
#19171 = CARTESIAN_POINT ( 'NONE',  ( -6.573387563318148885, 17.69612765735440973, -231.1211991061559274 ) ) ;
#19172 = EDGE_LOOP ( 'NONE', ( #3749, #15852 ) ) ;
#19173 =( NAMED_UNIT ( * ) SI_UNIT ( $, .STERADIAN. ) SOLID_ANGLE_UNIT ( ) );
#19174 = CARTESIAN_POINT ( 'NONE',  ( 12.58590500897257947, 11.38573988265384607, -230.4867078522624695 ) ) ;
#19175 = CARTESIAN_POINT ( 'NONE',  ( -28.08095947817005822, 1.343466879924336999, -219.1986237337335695 ) ) ;
#19176 = CARTESIAN_POINT ( 'NONE',  ( -23.54665576872953636, -14.78900941482413067, -230.7594827126482073 ) ) ;
#19177 = VECTOR ( 'NONE', #17996, 1000.000000000000000 ) ;
#19178 = CARTESIAN_POINT ( 'NONE',  ( 8.510712203779903007, -27.79691582975998898, -230.5316902582456180 ) ) ;
#19179 = CARTESIAN_POINT ( 'NONE',  ( -2.543684969149407227, 16.28137730373167713, -227.6987697727321915 ) ) ;
#19180 = CARTESIAN_POINT ( 'NONE',  ( 0.000000000000000000, 0.000000000000000000, -77.51594804401857175 ) ) ;
#19181 = CARTESIAN_POINT ( 'NONE',  ( 13.71585692689473213, 6.523039003617190801, -224.4540437369149402 ) ) ;
#19182 = CARTESIAN_POINT ( 'NONE',  ( -17.17400284685640344, 24.63223427531467280, -220.6313524368512162 ) ) ;
#19183 = CARTESIAN_POINT ( 'NONE',  ( -6.564517230509238743, 23.65597541655194647, -219.1225629381441991 ) ) ;
#19184 = ORIENTED_EDGE ( 'NONE', *, *, #10506, .F. ) ;
#19185 = CARTESIAN_POINT ( 'NONE',  ( 8.674175678922351196, 20.85307874897338110, -216.6688793998777101 ) ) ;
#19186 = CARTESIAN_POINT ( 'NONE',  ( -15.99768154740552717, 2.245235659047613908, -226.7015216759272107 ) ) ;
#19187 = CARTESIAN_POINT ( 'NONE',  ( 24.19672885113291727, 10.99915907690374439, -233.6834417629405891 ) ) ;
#19188 = CARTESIAN_POINT ( 'NONE',  ( 11.12240951639491549, -23.90857633046665853, -218.9373339142375130 ) ) ;
#19189 = PLANE ( 'NONE',  #1377 ) ;
#19190 = DIRECTION ( 'NONE',  ( -0.000000000000000000, -0.000000000000000000, -1.000000000000000000 ) ) ;
#19191 = CARTESIAN_POINT ( 'NONE',  ( -9.517741096562200909, 20.63709896626785678, -234.1036702156204967 ) ) ;
#19192 = CARTESIAN_POINT ( 'NONE',  ( -30.94549479715584539, -0.2777009447058255143, -220.3105931650466118 ) ) ;
#19193 = CARTESIAN_POINT ( 'NONE',  ( 22.03647168421188596, 0.3315607655626346961, -232.0572713672587213 ) ) ;
#19194 = CARTESIAN_POINT ( 'NONE',  ( 25.80927844399814930, 11.21489550116160316, -221.3538377621514996 ) ) ;
#19195 = CARTESIAN_POINT ( 'NONE',  ( -24.68906941503829700, 2.445024713909649705, -232.6803430500543755 ) ) ;
#19196 = CARTESIAN_POINT ( 'NONE',  ( 1.836136847161299990, -12.84546502099244591, -226.1727064218434293 ) ) ;
#19197 = CARTESIAN_POINT ( 'NONE',  ( -17.39699619235753048, 15.64332637722790054, -216.0406373264262641 ) ) ;
#19198 = VECTOR ( 'NONE', #6246, 1000.000000000000000 ) ;
#19199 = CARTESIAN_POINT ( 'NONE',  ( -13.01696012539752445, 9.878799299062107409, -218.8446158128127195 ) ) ;
#19200 = ORIENTED_EDGE ( 'NONE', *, *, #8422, .F. ) ;
#19201 = CARTESIAN_POINT ( 'NONE',  ( -18.08305592660031991, 4.022743421239192152, -217.2335041149100050 ) ) ;
#19202 = CARTESIAN_POINT ( 'NONE',  ( -22.54883021006152433, -16.50439104605484530, -230.5104955902558004 ) ) ;
#19203 = DIRECTION ( 'NONE',  ( -0.000000000000000000, -0.000000000000000000, -1.000000000000000000 ) ) ;
#19204 = CARTESIAN_POINT ( 'NONE',  ( -14.00380962569832199, 8.747390586476997854, -231.7950903513155936 ) ) ;
#19205 = CARTESIAN_POINT ( 'NONE',  ( 0.3839640804239903837, -16.65388496721540790, -217.3312339551772823 ) ) ;
#19206 = DIRECTION ( 'NONE',  ( 6.982962677686266711E-15, -1.000000000000000000, 0.000000000000000000 ) ) ;
#19207 = CARTESIAN_POINT ( 'NONE',  ( 18.76166303929372603, -2.999999999999992895, -225.1221413045205111 ) ) ;
#19208 = CARTESIAN_POINT ( 'NONE',  ( 20.41968681625622040, 10.18377600976054076, -218.1989382652844256 ) ) ;
#19209 = CARTESIAN_POINT ( 'NONE',  ( -4.558896566524145655, 13.01459016691503301, -228.3167740496058684 ) ) ;
#19210 = DIRECTION ( 'NONE',  ( 0.000000000000000000, 0.000000000000000000, -1.000000000000000000 ) ) ;
#19211 = CARTESIAN_POINT ( 'NONE',  ( 12.56556766396551872, 9.776144415819011613, -223.4791766911294815 ) ) ;
#19212 = CARTESIAN_POINT ( 'NONE',  ( 3.878020530997904114, -17.84699472038997214, -232.6985457136631794 ) ) ;
#19213 = ORIENTED_EDGE ( 'NONE', *, *, #18602, .T. ) ;
#19214 = CARTESIAN_POINT ( 'NONE',  ( -4.490213599459100813, 14.55066867058898694, -222.6488251579668827 ) ) ;
#19215 = CARTESIAN_POINT ( 'NONE',  ( -15.82760502346409304, 5.624826830110399634, -227.5369622385896946 ) ) ;
#19216 = CARTESIAN_POINT ( 'NONE',  ( -24.79170285622992509, 4.551775110860766915, -234.5907228154019322 ) ) ;
#19217 = AXIS2_PLACEMENT_3D ( 'NONE', #9279, #14453, #2175 ) ;
#19218 = CARTESIAN_POINT ( 'NONE',  ( -16.83358080157556103, -19.16169236771116857, -229.6922051654298116 ) ) ;
#19219 = DIRECTION ( 'NONE',  ( 0.000000000000000000, 0.000000000000000000, -1.000000000000000000 ) ) ;
#19220 = ORIENTED_EDGE ( 'NONE', *, *, #16998, .T. ) ;
#19221 = PRESENTATION_LAYER_ASSIGNMENT (  '', '', ( #7747 ) ) ;
#19222 = CARTESIAN_POINT ( 'NONE',  ( 24.34047711160105720, 17.90454708687460794, -228.1939002122307159 ) ) ;
#19223 = CARTESIAN_POINT ( 'NONE',  ( 7.436546160899932367, -15.25288503996851475, -221.8354696069030467 ) ) ;
#19224 = CARTESIAN_POINT ( 'NONE',  ( 12.23063869552301242, 12.84118223717021934, -218.8273164334868284 ) ) ;
#19225 = ADVANCED_FACE ( 'NONE', ( #20804 ), #13965, .F. ) ;
#19226 = CARTESIAN_POINT ( 'NONE',  ( -11.02345917017863464, 29.02019856777526741, -223.9475008740665771 ) ) ;
#19227 = CARTESIAN_POINT ( 'NONE',  ( 29.96674103997387206, 4.060923908484647349, -228.5323681967686298 ) ) ;
#19228 = CARTESIAN_POINT ( 'NONE',  ( 7.995304978256253747, 13.28024228361502779, -220.6535174700288451 ) ) ;
#19229 = DIRECTION ( 'NONE',  ( 1.000000000000000000, 0.000000000000000000, 0.000000000000000000 ) ) ;
#19230 = CARTESIAN_POINT ( 'NONE',  ( -8.376153411442972541, -27.59911039556260448, -219.0729038785590888 ) ) ;
#19231 = CARTESIAN_POINT ( 'NONE',  ( 9.104026917753444081, -10.66572815660443041, -221.9193219976906448 ) ) ;
#19232 = CARTESIAN_POINT ( 'NONE',  ( 0.000000000000000000, 0.000000000000000000, -77.51594804401857175 ) ) ;
#19233 = CARTESIAN_POINT ( 'NONE',  ( 0.000000000000000000, 0.000000000000000000, -105.0000000000000000 ) ) ;
#19234 = CARTESIAN_POINT ( 'NONE',  ( -20.06846544527470400, 7.877362284741439069, -235.3910773253824402 ) ) ;
#19235 = CARTESIAN_POINT ( 'NONE',  ( -20.58881354142085485, -10.73024182470851606, -219.1570184730780397 ) ) ;
#19236 = CARTESIAN_POINT ( 'NONE',  ( 13.98152565379061052, 2.156981915107639036, -230.5667344709999611 ) ) ;
#19237 = CARTESIAN_POINT ( 'NONE',  ( 2.630208337444488453, 16.40323635460054774, -219.2570070657488088 ) ) ;
#19238 = CARTESIAN_POINT ( 'NONE',  ( -1.316322971969275502, 14.13179993441458215, -224.9782367179667233 ) ) ;
#19239 = EDGE_LOOP ( 'NONE', ( #13295, #1889, #7942, #20418 ) ) ;
#19240 = CARTESIAN_POINT ( 'NONE',  ( 14.43570356028121893, -19.75277720499002498, -215.7015347705405759 ) ) ;
#19241 = ORIENTED_EDGE ( 'NONE', *, *, #17683, .T. ) ;
#19242 = CARTESIAN_POINT ( 'NONE',  ( 26.24002132888527328, 11.62331517472360964, -222.5300873157218859 ) ) ;
#19243 = CARTESIAN_POINT ( 'NONE',  ( -8.995433708001568718, 13.44373928221519243, -231.9251680978426577 ) ) ;
#19244 = EDGE_CURVE ( 'NONE', #20783, #16621, #1878, .T. ) ;
#19245 = CARTESIAN_POINT ( 'NONE',  ( -15.51814470728089645, 2.949994979016113739, -222.8331727603033130 ) ) ;
#19246 = CARTESIAN_POINT ( 'NONE',  ( -14.33274213004767716, -3.240524307521291725, -229.5155949954044559 ) ) ;
#19247 = CARTESIAN_POINT ( 'NONE',  ( -17.39699619235753048, 15.64332637722790054, -216.0406373264262641 ) ) ;
#19248 = FACE_OUTER_BOUND ( 'NONE', #3879, .T. ) ;
#19249 = CIRCLE ( 'NONE', #9559, 13.12488928717151637 ) ;
#19250 = CARTESIAN_POINT ( 'NONE',  ( 14.68028918641733149, -3.003797161868758447, -225.1263072288626006 ) ) ;
#19251 = FACE_OUTER_BOUND ( 'NONE', #1196, .T. ) ;
#19252 = CARTESIAN_POINT ( 'NONE',  ( -17.75632171729475317, 14.45153669854845901, -218.6240360064753929 ) ) ;
#19253 = CARTESIAN_POINT ( 'NONE',  ( 17.85905871012913693, 8.463974683125162102, -234.6532732619751300 ) ) ;
#19254 = CARTESIAN_POINT ( 'NONE',  ( 16.40130693394614525, -0.1574073183566240264, -221.9481963320051534 ) ) ;
#19255 = CARTESIAN_POINT ( 'NONE',  ( -17.53163374842703703, -10.16025041587072764, -214.8411325589202647 ) ) ;
#19256 = CARTESIAN_POINT ( 'NONE',  ( -21.27082149447729620, -6.316573346028001801, -216.2864220516500779 ) ) ;
#19257 = CARTESIAN_POINT ( 'NONE',  ( -7.903959818038710061, 11.02445096303677552, -229.5951168968472871 ) ) ;
#19258 = CARTESIAN_POINT ( 'NONE',  ( -14.24095617957673632, -25.86326826095433162, -229.7068514753157160 ) ) ;
#19259 = CARTESIAN_POINT ( 'NONE',  ( 4.656903975822286768, 13.45000048768594780, -227.6722060245555497 ) ) ;
#19260 = CARTESIAN_POINT ( 'NONE',  ( 6.571750410407496190, -24.62545695199335682, -234.5391748598602248 ) ) ;
#19261 = AXIS2_PLACEMENT_3D ( 'NONE', #3950, #3841, #10722 ) ;
#19262 = CARTESIAN_POINT ( 'NONE',  ( 22.91388766833460977, -2.807094692329320838E-15, -75.05807060175870049 ) ) ;
#19263 = CARTESIAN_POINT ( 'NONE',  ( 28.53243699394185384, 6.329221954355706004, -218.6437889135959267 ) ) ;
#19264 = SURFACE_SIDE_STYLE ('',( #20946 ) ) ;
#19265 = CARTESIAN_POINT ( 'NONE',  ( -2.618694198633108261, 15.69630225547860825, -226.1451761977223498 ) ) ;
#19266 = CARTESIAN_POINT ( 'NONE',  ( -24.79507334250576278, 6.844873424762779379, -218.1074956078844878 ) ) ;
#19267 = CARTESIAN_POINT ( 'NONE',  ( 27.40550551777678123, 5.967061366481472895, -228.7463788799179554 ) ) ;
#19268 = CARTESIAN_POINT ( 'NONE',  ( 29.81944548462877975, 8.043843257819576209, -228.1755181449411793 ) ) ;
#19269 = CARTESIAN_POINT ( 'NONE',  ( -15.00281653375496127, -15.21317112889928858, -231.9690514080965613 ) ) ;
#19270 = AXIS2_PLACEMENT_3D ( 'NONE', #19083, #10542, #14040 ) ;
#19271 = CARTESIAN_POINT ( 'NONE',  ( 16.71363093372661979, 20.70203100498337179, -215.6856694095356488 ) ) ;
#19272 = DIRECTION ( 'NONE',  ( 0.000000000000000000, 0.000000000000000000, -1.000000000000000000 ) ) ;
#19273 = CARTESIAN_POINT ( 'NONE',  ( -14.25383187134801588, -24.74900029534085633, -216.9920501705437630 ) ) ;
#19274 = CARTESIAN_POINT ( 'NONE',  ( -4.386767007475907754, 14.39570986262862107, -223.2690175027443615 ) ) ;
#19275 = TOROIDAL_SURFACE ( 'NONE', #4898, 22.63401512838748175, 3.000000000000002665 ) ;
#19276 = CARTESIAN_POINT ( 'NONE',  ( 10.12956299421491302, 11.38773431477224385, -230.3175791991728829 ) ) ;
#19277 = ADVANCED_FACE ( 'NONE', ( #14077 ), #7434, .F. ) ;
#19278 = CARTESIAN_POINT ( 'NONE',  ( -21.26441444091935296, 10.69428164102106926, -219.3434466924981336 ) ) ;
#19279 = CARTESIAN_POINT ( 'NONE',  ( -11.59874896804548250, 27.28969409813203484, -218.8626241359735332 ) ) ;
#19280 = CARTESIAN_POINT ( 'NONE',  ( 14.64440749032966593, 2.523901497798496596, -225.4572725674553340 ) ) ;
#19281 = CARTESIAN_POINT ( 'NONE',  ( 7.724698117049915602, -20.76727510557136469, -231.0612438369181518 ) ) ;
#19282 = EDGE_LOOP ( 'NONE', ( #21558, #11439, #19934, #9165 ) ) ;
#19283 = CARTESIAN_POINT ( 'NONE',  ( 6.025688374458400887, -15.61258154445926749, -220.0079782759978002 ) ) ;
#19284 = CARTESIAN_POINT ( 'NONE',  ( -2.015708574708954259, 26.78900769828807782, -221.5371848586876808 ) ) ;
#19285 = ORIENTED_EDGE ( 'NONE', *, *, #1027, .T. ) ;
#19286 = FACE_OUTER_BOUND ( 'NONE', #13244, .T. ) ;
#19287 = CARTESIAN_POINT ( 'NONE',  ( 7.639528166734322667, 11.92751229241157596, -224.6077814063189635 ) ) ;
#19288 = CARTESIAN_POINT ( 'NONE',  ( 25.69761320619099720, -8.403105518750903613, -219.2599777650661110 ) ) ;
#19289 = CARTESIAN_POINT ( 'NONE',  ( -11.49803752765619258, -8.459563989871591971, -222.4296168992866853 ) ) ;
#19290 = CARTESIAN_POINT ( 'NONE',  ( 0.5120693878963755719, -30.63998626839889639, -227.9504769009175220 ) ) ;
#19291 = CARTESIAN_POINT ( 'NONE',  ( 0.9458336400950161371, 17.49535648476021876, -228.8359568483051589 ) ) ;
#19292 = DIRECTION ( 'NONE',  ( 0.000000000000000000, -1.000000000000000000, 0.000000000000000000 ) ) ;
#19293 = CARTESIAN_POINT ( 'NONE',  ( 25.53003411612920459, 7.940385729200389875, -230.5495695598654322 ) ) ;
#19294 = CARTESIAN_POINT ( 'NONE',  ( -7.395406416482832590, 12.93623984139929739, -219.2606224730616873 ) ) ;
#19295 = CARTESIAN_POINT ( 'NONE',  ( -2.618694198633108261, 15.69630225547860825, -226.1451761977223498 ) ) ;
#19296 = EDGE_LOOP ( 'NONE', ( #14083, #14579, #14361, #17608 ) ) ;
#19297 = CARTESIAN_POINT ( 'NONE',  ( 0.3632086708616291126, 21.06287758167331958, -232.5112839711303820 ) ) ;
#19298 = CARTESIAN_POINT ( 'NONE',  ( -15.65611835717891687, 5.486779671999271635, -227.0554626315911264 ) ) ;
#19299 = CARTESIAN_POINT ( 'NONE',  ( 29.33969601628096768, 11.98971187598327504, -225.2039690377576733 ) ) ;
#19300 = CARTESIAN_POINT ( 'NONE',  ( 7.092430827040528740, -27.48041265710635628, -228.4891580147104548 ) ) ;
#19301 = DIRECTION ( 'NONE',  ( 1.000000000000000000, 0.000000000000000000, 0.000000000000000000 ) ) ;
#19302 = ORIENTED_EDGE ( 'NONE', *, *, #15198, .T. ) ;
#19303 = CARTESIAN_POINT ( 'NONE',  ( 12.10245006109274080, 26.02147364279441888, -220.6079829738538649 ) ) ;
#19304 = CARTESIAN_POINT ( 'NONE',  ( 25.61231557635624156, -8.129803667132245337, -228.3450084804328242 ) ) ;
#19305 = FACE_OUTER_BOUND ( 'NONE', #16030, .T. ) ;
#19306 = CARTESIAN_POINT ( 'NONE',  ( 19.20300624114736721, 0.6066039755357417462, -231.5046416827383950 ) ) ;
#19307 = CARTESIAN_POINT ( 'NONE',  ( 8.709470447750865318, -17.43408031369701661, -216.5121658579468829 ) ) ;
#19308 = DIRECTION ( 'NONE',  ( 0.000000000000000000, 0.000000000000000000, 1.000000000000000000 ) ) ;
#19309 = CARTESIAN_POINT ( 'NONE',  ( -6.201839134465864767, 11.37481922992157379, -223.7040893475979146 ) ) ;
#19310 = CARTESIAN_POINT ( 'NONE',  ( -19.61183938075907918, 22.25855138946451106, -229.5731876748794207 ) ) ;
#19311 = ORIENTED_EDGE ( 'NONE', *, *, #3598, .T. ) ;
#19312 = CARTESIAN_POINT ( 'NONE',  ( 21.83031488337932657, -1.542591969257240070, -231.3901500139511427 ) ) ;
#19313 = CARTESIAN_POINT ( 'NONE',  ( -11.18311023676720062, -15.30649302686804347, -231.8766562234714002 ) ) ;
#19314 = CARTESIAN_POINT ( 'NONE',  ( 0.000000000000000000, 0.000000000000000000, 95.00000000000000000 ) ) ;
#19315 = CARTESIAN_POINT ( 'NONE',  ( 25.50000000000000000, 0.5000000000000000000, 0.000000000000000000 ) ) ;
#19316 = CARTESIAN_POINT ( 'NONE',  ( -29.88125065636863198, 4.504452993877526623, -226.2048141718237275 ) ) ;
#19317 = CARTESIAN_POINT ( 'NONE',  ( 0.4504461526642338232, -19.62726417856956473, -215.9916429883993487 ) ) ;
#19318 = CARTESIAN_POINT ( 'NONE',  ( 0.000000000000000000, 0.000000000000000000, 75.00000000000000000 ) ) ;
#19319 = CARTESIAN_POINT ( 'NONE',  ( 19.67070349224072956, 16.44307963282299312, -220.0378483479504439 ) ) ;
#19320 = EDGE_CURVE ( 'NONE', #18628, #8679, #448, .T. ) ;
#19321 = CARTESIAN_POINT ( 'NONE',  ( -16.13584396029534318, 23.78382729893626646, -231.6788043429177435 ) ) ;
#19322 = DIRECTION ( 'NONE',  ( -0.000000000000000000, -0.000000000000000000, 1.000000000000000000 ) ) ;
#19323 = CARTESIAN_POINT ( 'NONE',  ( 11.73428189025226942, 12.46434742632455084, -228.1539301014595083 ) ) ;
#19324 = CARTESIAN_POINT ( 'NONE',  ( -3.821460206879919941, -14.75247343660110921, -225.5705290259156470 ) ) ;
#19325 = ORIENTED_EDGE ( 'NONE', *, *, #14070, .T. ) ;
#19326 = EDGE_CURVE ( 'NONE', #21555, #10013, #458, .T. ) ;
#19327 = CARTESIAN_POINT ( 'NONE',  ( -4.142636420702924482, 14.17169704882741321, -225.1666440184957310 ) ) ;
#19328 = CARTESIAN_POINT ( 'NONE',  ( -9.679547659771646551, 14.60131434979866505, -230.4338124916943968 ) ) ;
#19329 = CARTESIAN_POINT ( 'NONE',  ( 19.10353041285295816, 2.510539514498965730, -232.1135168369976896 ) ) ;
#19330 = CARTESIAN_POINT ( 'NONE',  ( -16.75383819933101748, -8.593015344009392820, -230.3978590765929084 ) ) ;
#19331 = CARTESIAN_POINT ( 'NONE',  ( -25.00000000000000000, 0.000000000000000000, 75.00000000000000000 ) ) ;
#19332 = ORIENTED_EDGE ( 'NONE', *, *, #9202, .T. ) ;
#19333 = CARTESIAN_POINT ( 'NONE',  ( 20.88210880980788531, 0.9259446317980322139, -218.6312544800709929 ) ) ;
#19334 = CARTESIAN_POINT ( 'NONE',  ( 3.191506000329551007, -19.56356538597602679, -231.2193641236077326 ) ) ;
#19335 = CARTESIAN_POINT ( 'NONE',  ( 12.58590500897257947, 11.38573988265384607, -230.4867078522624695 ) ) ;
#19336 = CARTESIAN_POINT ( 'NONE',  ( -3.514547081416551588, 30.38636916157537016, -227.3529586180979436 ) ) ;
#19337 = CARTESIAN_POINT ( 'NONE',  ( 13.12946830070648652, 6.370976456471619365, -231.5124810213676483 ) ) ;
#19338 = CARTESIAN_POINT ( 'NONE',  ( 12.18657022793382794, 26.76558097653315471, -221.8882195427397335 ) ) ;
#19339 = CARTESIAN_POINT ( 'NONE',  ( 13.45723858497841618, 1.555143580403207659, -222.4309038978887543 ) ) ;
#19340 = CARTESIAN_POINT ( 'NONE',  ( -21.52428768452188734, -21.65989873160339840, -225.4304055049964006 ) ) ;
#19341 = CARTESIAN_POINT ( 'NONE',  ( 19.06435866915521515, -20.24829071055443563, -218.8318535520223804 ) ) ;
#19342 = DIRECTION ( 'NONE',  ( 0.000000000000000000, 0.000000000000000000, -1.000000000000000000 ) ) ;
#19343 = LINE ( 'NONE', #20697, #10159 ) ;
#19344 = CARTESIAN_POINT ( 'NONE',  ( -29.15345109632842124, 14.07532767497844262, -225.0972140442887621 ) ) ;
#19345 = CARTESIAN_POINT ( 'NONE',  ( -25.33517302999029042, -8.734563104097837538, -228.3677567689655916 ) ) ;
#19346 = CARTESIAN_POINT ( 'NONE',  ( -22.38347148959098121, 12.58966534755613687, -218.4978713241202399 ) ) ;
#19347 = CARTESIAN_POINT ( 'NONE',  ( 14.63115627273841923, 9.024791562541032874, -232.5054678133655841 ) ) ;
#19348 = CARTESIAN_POINT ( 'NONE',  ( 5.104697752190542559, 17.18208638613223016, -220.3923334988619445 ) ) ;
#19349 = ORIENTED_EDGE ( 'NONE', *, *, #13826, .T. ) ;
#19350 = CARTESIAN_POINT ( 'NONE',  ( 13.82710435306955432, -11.68840971183345800, -215.7775723145259974 ) ) ;
#19351 = VERTEX_POINT ( 'NONE', #8670 ) ;
#19352 = CARTESIAN_POINT ( 'NONE',  ( 20.34032485158648029, 2.741617426884598530, -217.9827731991294968 ) ) ;
#19353 = CARTESIAN_POINT ( 'NONE',  ( -13.66744685701839046, 5.938820276054873837, -223.0954633396572149 ) ) ;
#19354 = CARTESIAN_POINT ( 'NONE',  ( -10.01410430826631170, 16.10970239316000630, -233.6135099156378203 ) ) ;
#19355 = CARTESIAN_POINT ( 'NONE',  ( -13.83093441725390704, -7.146379636134302160, -230.0501880019394605 ) ) ;
#19356 = CARTESIAN_POINT ( 'NONE',  ( -15.20262116893801974, 8.038155052917188570, -217.6767387945475036 ) ) ;
#19357 = TOROIDAL_SURFACE ( 'NONE', #20422, 13.12488928717151637, 5.000000000000000000 ) ;
#19358 = CARTESIAN_POINT ( 'NONE',  ( 0.000000000000000000, 0.000000000000000000, -24.99999999999999645 ) ) ;
#19359 = CARTESIAN_POINT ( 'NONE',  ( 14.62702828724412285, -1.994068170757606673, -224.0552340365271959 ) ) ;
#19360 = CARTESIAN_POINT ( 'NONE',  ( -11.82020046940938407, 10.16362659047642758, -224.3364193436540575 ) ) ;
#19361 = CARTESIAN_POINT ( 'NONE',  ( 13.34963947135311102, 7.416462695144936390, -217.9359469527792044 ) ) ;
#19362 = CARTESIAN_POINT ( 'NONE',  ( 16.56146809408446430, -0.9616313295950813522, -228.5729530379900609 ) ) ;
#19363 = CARTESIAN_POINT ( 'NONE',  ( 10.55627441269396094, 10.31758739525044888, -223.1990319438957613 ) ) ;
#19364 = CARTESIAN_POINT ( 'NONE',  ( -14.80115690555879659, -8.758261077448048937, -218.2925738755452016 ) ) ;
#19365 = CARTESIAN_POINT ( 'NONE',  ( -2.125813515909480866, 15.68152656492264363, -220.3943115937447317 ) ) ;
#19366 = CARTESIAN_POINT ( 'NONE',  ( -1.633632075387274840, -15.48245080501611071, -218.5193615163172751 ) ) ;
#19367 = CARTESIAN_POINT ( 'NONE',  ( 7.168644370073567806, 19.32044210858112265, -233.1278450877711634 ) ) ;
#19368 = CARTESIAN_POINT ( 'NONE',  ( 5.917072789534883803, -21.18442853552521754, -235.1867574136372525 ) ) ;
#19369 = CARTESIAN_POINT ( 'NONE',  ( 1.322875655532295136, 1.500000000000000000, -120.0000000000000142 ) ) ;
#19370 = CARTESIAN_POINT ( 'NONE',  ( -10.02095171162140019, 11.02119725306997111, -224.1251327387667516 ) ) ;
#19371 = SURFACE_SIDE_STYLE ('',( #10940 ) ) ;
#19372 = CARTESIAN_POINT ( 'NONE',  ( 27.12528000378512871, -1.050705938820645224, -232.4139529590446784 ) ) ;
#19373 = CARTESIAN_POINT ( 'NONE',  ( 3.614175329767659761, 21.98488100320606264, -219.0898850257099753 ) ) ;
#19374 = CARTESIAN_POINT ( 'NONE',  ( 14.55590852435181226, 2.816890518231522034, -218.5131513550309990 ) ) ;
#19375 = CARTESIAN_POINT ( 'NONE',  ( 17.34727976380017722, 4.822939981779328811, -230.8836217450937909 ) ) ;
#19376 = CARTESIAN_POINT ( 'NONE',  ( -7.753256282497156704, -15.05334625439219565, -219.2728364670455221 ) ) ;
#19377 = CARTESIAN_POINT ( 'NONE',  ( 10.66732316618037402, 25.78610527446713263, -216.5597036843431624 ) ) ;
#19378 = DIRECTION ( 'NONE',  ( 0.000000000000000000, 0.000000000000000000, 1.000000000000000000 ) ) ;
#19379 = CARTESIAN_POINT ( 'NONE',  ( -6.154316005079235374, -31.08134634390615503, -226.4265589226172892 ) ) ;
#19380 = CARTESIAN_POINT ( 'NONE',  ( -11.03778527004271659, 26.96286968643956428, -225.4057095641571209 ) ) ;
#19381 = CARTESIAN_POINT ( 'NONE',  ( 22.73582563804385970, 20.20868311426415431, -227.8513184012435886 ) ) ;
#19382 = CARTESIAN_POINT ( 'NONE',  ( -24.82235633397527508, 10.76243500821901300, -227.9886044494091948 ) ) ;
#19383 = CARTESIAN_POINT ( 'NONE',  ( 4.569118550756183339, 31.72363458735121000, -222.3920438419263519 ) ) ;
#19384 = CARTESIAN_POINT ( 'NONE',  ( 27.84414217501293010, 2.965433895642837214, -221.8999927093654492 ) ) ;
#19385 = CARTESIAN_POINT ( 'NONE',  ( 6.592356972974974916, -14.93599889844929862, -226.9608163220883625 ) ) ;
#19386 = ORIENTED_EDGE ( 'NONE', *, *, #6802, .F. ) ;
#19387 = CARTESIAN_POINT ( 'NONE',  ( 9.835929410207317147, -16.71508016877321268, -232.2716196330763694 ) ) ;
#19388 = CARTESIAN_POINT ( 'NONE',  ( -10.30040261405712698, 19.75576125044891285, -218.0811964201226658 ) ) ;
#19389 = CARTESIAN_POINT ( 'NONE',  ( 0.000000000000000000, -23.00000000000006040, -75.00000000000000000 ) ) ;
#19390 = CARTESIAN_POINT ( 'NONE',  ( 15.87442104186276381, 8.674488492264579520, -230.9702037640878416 ) ) ;
#19391 = CARTESIAN_POINT ( 'NONE',  ( 14.56914850832129815, -2.041740472307377985, -224.7121590863160350 ) ) ;
#19392 = CARTESIAN_POINT ( 'NONE',  ( -22.23616899077527975, -11.51447210886970751, -217.5950109096934568 ) ) ;
#19393 = CARTESIAN_POINT ( 'NONE',  ( -7.460068573003235670, -29.58770008691625364, -228.1902472473001637 ) ) ;
#19394 = CARTESIAN_POINT ( 'NONE',  ( -3.010752168931037698, 15.84372070116375575, -223.4060793985500482 ) ) ;
#19395 = CARTESIAN_POINT ( 'NONE',  ( 23.03038449397558196, 0.000000000000000000, 75.34729635533385306 ) ) ;
#19396 = CARTESIAN_POINT ( 'NONE',  ( 24.52860916307685457, 12.75391509163817361, -221.3604763108436941 ) ) ;
#19397 = CARTESIAN_POINT ( 'NONE',  ( -4.104500432947460808, 15.73223271406093460, -218.0734292856946297 ) ) ;
#19398 = CARTESIAN_POINT ( 'NONE',  ( 3.689800395305025127, 23.07294874520714956, -219.2515233573129478 ) ) ;
#19399 = EDGE_LOOP ( 'NONE', ( #2463, #16910, #22066, #23 ) ) ;
#19400 = CARTESIAN_POINT ( 'NONE',  ( 10.31623634631035991, 26.83927646318382898, -220.2315638557092541 ) ) ;
#19401 = CARTESIAN_POINT ( 'NONE',  ( 13.30790133003807441, 0.6370684082013071681, -222.3495379725305270 ) ) ;
#19402 = CARTESIAN_POINT ( 'NONE',  ( 15.65443801613259467, 7.488839228060037989, -233.6469817377710569 ) ) ;
#19403 = CARTESIAN_POINT ( 'NONE',  ( 10.05661706967825353, -14.25456047934742365, -218.9909083857680230 ) ) ;
#19404 = CARTESIAN_POINT ( 'NONE',  ( 21.96352831578809273, -0.3315607655629317918, -233.9427286327412503 ) ) ;
#19405 = CARTESIAN_POINT ( 'NONE',  ( -19.79999999999999716, 0.000000000000000000, 78.50000000000000000 ) ) ;
#19406 = CARTESIAN_POINT ( 'NONE',  ( 10.66614775643814994, 26.29080367171353672, -230.0818785118670178 ) ) ;
#19407 = CARTESIAN_POINT ( 'NONE',  ( 21.58416078958130413, -8.344710983103166058, -219.2549068428508861 ) ) ;
#19408 = LINE ( 'NONE', #2307, #2932 ) ;
#19409 = CARTESIAN_POINT ( 'NONE',  ( 13.47054497134856277, -24.75371201277411615, -218.7687119198782000 ) ) ;
#19410 = CARTESIAN_POINT ( 'NONE',  ( -10.84997096467605182, 25.01800101807719301, -232.4518260228253155 ) ) ;
#19411 = CARTESIAN_POINT ( 'NONE',  ( -11.94727018630768178, 9.025563988971828877, -220.6148682757971358 ) ) ;
#19412 = ORIENTED_EDGE ( 'NONE', *, *, #20644, .F. ) ;
#19413 = CARTESIAN_POINT ( 'NONE',  ( -17.17400284685640344, 24.63223427531467280, -220.6313524368512162 ) ) ;
#19414 = CARTESIAN_POINT ( 'NONE',  ( -21.50522087930578152, -16.03150550247721640, -231.4768288373508369 ) ) ;
#19415 = DIRECTION ( 'NONE',  ( -0.000000000000000000, 6.938893903907222461E-16, -1.000000000000000000 ) ) ;
#19416 = DIRECTION ( 'NONE',  ( -0.000000000000000000, -0.000000000000000000, -1.000000000000000000 ) ) ;
#19417 = CARTESIAN_POINT ( 'NONE',  ( -15.15110768032078070, 3.517015312212880218, -219.5479300368539270 ) ) ;
#19418 = CARTESIAN_POINT ( 'NONE',  ( 9.471595414968767557, -23.22249338881061931, -232.1368331642201497 ) ) ;
#19419 = CARTESIAN_POINT ( 'NONE',  ( -18.47334320050258327, 24.79293862780133040, -226.9986786077537317 ) ) ;
#19420 = CARTESIAN_POINT ( 'NONE',  ( 25.18311526135610734, 13.65721788432563955, -224.7326014392022273 ) ) ;
#19421 = CARTESIAN_POINT ( 'NONE',  ( -7.903959818038710061, 11.02445096303677552, -229.5951168968472871 ) ) ;
#19422 = PLANE ( 'NONE',  #1544 ) ;
#19423 = CARTESIAN_POINT ( 'NONE',  ( 14.12692363916921146, 20.59586666873830296, -230.0804552526094540 ) ) ;
#19424 = CARTESIAN_POINT ( 'NONE',  ( -3.088421015035204498, -25.33386621341791667, -218.8172537214380498 ) ) ;
#19425 = AXIS2_PLACEMENT_3D ( 'NONE', #5905, #4427, #4316 ) ;
#19426 = EDGE_CURVE ( 'NONE', #7596, #11, #1529, .T. ) ;
#19427 = ORIENTED_EDGE ( 'NONE', *, *, #3630, .T. ) ;
#19428 = CARTESIAN_POINT ( 'NONE',  ( -10.84440549681320221, 27.00404139634608214, -224.0969657459751261 ) ) ;
#19429 = CARTESIAN_POINT ( 'NONE',  ( -9.852301241816233457, 15.10013604187968461, -230.8124578431014697 ) ) ;
#19430 = CARTESIAN_POINT ( 'NONE',  ( -15.72555926117677139, 17.60926865496976745, -217.2114552733360142 ) ) ;
#19431 = CARTESIAN_POINT ( 'NONE',  ( -12.22799442060091657, -11.48557521842085372, -222.2662941369099201 ) ) ;
#19432 = CYLINDRICAL_SURFACE ( 'NONE', #18290, 23.00000000000000000 ) ;
#19433 = ORIENTED_EDGE ( 'NONE', *, *, #1141, .F. ) ;
#19434 = CARTESIAN_POINT ( 'NONE',  ( -13.65925618638770800, 3.289586759644148817, -222.1579143493116533 ) ) ;
#19435 = CARTESIAN_POINT ( 'NONE',  ( 3.849154133940814848, -15.34907234289524958, -223.0340372416051196 ) ) ;
#19436 = CARTESIAN_POINT ( 'NONE',  ( 25.33562512631297281, 12.25422971834577268, -228.6777356031426791 ) ) ;
#19437 = CARTESIAN_POINT ( 'NONE',  ( -4.620781219515533778, 16.99182040716223696, -217.1278208835672672 ) ) ;
#19438 = EDGE_CURVE ( 'NONE', #9979, #4726, #19343, .T. ) ;
#19439 = CARTESIAN_POINT ( 'NONE',  ( -18.91027996815576628, 5.295101183552822555, -231.2253513302548527 ) ) ;
#19440 = CARTESIAN_POINT ( 'NONE',  ( 7.393167209263542539, 10.77319710117329699, -221.1179833906701049 ) ) ;
#19441 = CARTESIAN_POINT ( 'NONE',  ( 14.32085100525799248, 9.220655089380342062, -219.9006227404039464 ) ) ;
#19442 = CARTESIAN_POINT ( 'NONE',  ( 13.54927135793711557, 0.6749664302445949060, -222.0769159577524192 ) ) ;
#19443 = CARTESIAN_POINT ( 'NONE',  ( -21.63546480557098306, -21.44004028177477750, -223.8762611443524122 ) ) ;
#19444 = CARTESIAN_POINT ( 'NONE',  ( 8.257114973007913861, -25.39836461225790742, -232.6217252414676295 ) ) ;
#19445 = DIRECTION ( 'NONE',  ( -1.000000000000000000, 0.000000000000000000, 0.000000000000000000 ) ) ;
#19446 = DIRECTION ( 'NONE',  ( 1.000000000000000000, 0.000000000000000000, 0.000000000000000000 ) ) ;
#19447 = CARTESIAN_POINT ( 'NONE',  ( -24.77996431573922820, 10.49354383977773786, -234.1655613096203581 ) ) ;
#19448 = CARTESIAN_POINT ( 'NONE',  ( -15.58915292315067802, -7.289217648355976742, -221.6802381019405175 ) ) ;
#19449 = CARTESIAN_POINT ( 'NONE',  ( -26.19327040236159831, 13.44417515682194875, -223.7810975255189874 ) ) ;
#19450 = CARTESIAN_POINT ( 'NONE',  ( 11.98894270675143225, 20.38243841428667835, -233.2283128908360084 ) ) ;
#19451 = CARTESIAN_POINT ( 'NONE',  ( -1.973645837583506424, 28.78841935349527503, -228.5341874691134763 ) ) ;
#19452 = ORIENTED_EDGE ( 'NONE', *, *, #6515, .T. ) ;
#19453 = CARTESIAN_POINT ( 'NONE',  ( 22.53017539111736411, -13.33152463597901516, -234.4848520764015518 ) ) ;
#19454 = CARTESIAN_POINT ( 'NONE',  ( 16.64225601860865211, 1.926018578292457928, -220.2177910260893725 ) ) ;
#19455 = VECTOR ( 'NONE', #12118, 1000.000000000000000 ) ;
#19456 = CARTESIAN_POINT ( 'NONE',  ( 0.1645309800062008665, 15.56029994314186382, -233.1129172884685943 ) ) ;
#19457 = CARTESIAN_POINT ( 'NONE',  ( -19.98042543492610079, 23.51949599776966693, -226.6701036947414138 ) ) ;
#19458 = CARTESIAN_POINT ( 'NONE',  ( -26.76734473129764069, -3.453818734898710829, -232.3222361544058003 ) ) ;
#19459 = CARTESIAN_POINT ( 'NONE',  ( -28.13472254077564116, 12.33996625515159629, -224.9141344439281909 ) ) ;
#19460 = CARTESIAN_POINT ( 'NONE',  ( -12.40805626191516708, -7.677656142228116209, 93.00000000000000000 ) ) ;
#19461 = CARTESIAN_POINT ( 'NONE',  ( 26.54225689383817866, -6.924125931238839016, -230.1506921200174247 ) ) ;
#19462 = AXIS2_PLACEMENT_3D ( 'NONE', #10479, #21043, #5518 ) ;
#19463 = CARTESIAN_POINT ( 'NONE',  ( 3.001892273201697048, 27.20292285420111966, -216.7800154582108689 ) ) ;
#19464 = CARTESIAN_POINT ( 'NONE',  ( 13.40064012097826307, 2.532414129335418096, -221.5952957478750989 ) ) ;
#19465 = CARTESIAN_POINT ( 'NONE',  ( 15.57986488780344736, -0.6155558446892130942, -225.2777919203616932 ) ) ;
#19466 = CARTESIAN_POINT ( 'NONE',  ( 12.99034161053428349, 11.71468708507361889, -230.9043293568357740 ) ) ;
#19467 = CIRCLE ( 'NONE', #18412, 23.00000000000000000 ) ;
#19468 = CARTESIAN_POINT ( 'NONE',  ( -15.33992272861872763, -7.600289318192222865, -231.6130094852651951 ) ) ;
#19469 = EDGE_LOOP ( 'NONE', ( #6401, #3905, #21451, #10273 ) ) ;
#19470 = CARTESIAN_POINT ( 'NONE',  ( 5.563568780623874943, 21.86458082533069103, -218.6474243140849012 ) ) ;
#19471 = CARTESIAN_POINT ( 'NONE',  ( -5.178973235464019886, -24.35492185057628944, -233.6431870320687381 ) ) ;
#19472 = CARTESIAN_POINT ( 'NONE',  ( 4.389496648589924277, 14.47660514356954131, -220.6151178996808540 ) ) ;
#19473 = CARTESIAN_POINT ( 'NONE',  ( 6.679393088666140343, -31.31585170264869689, -224.7195491891107793 ) ) ;
#19474 = CARTESIAN_POINT ( 'NONE',  ( 14.30360180157784988, -0.2838691938953850080, -227.9870050950131315 ) ) ;
#19475 = CARTESIAN_POINT ( 'NONE',  ( -16.74094048923576494, 16.03040267675914521, -217.9177456399057178 ) ) ;
#19476 = DIRECTION ( 'NONE',  ( 0.000000000000000000, 0.000000000000000000, 1.000000000000000000 ) ) ;
#19477 = CARTESIAN_POINT ( 'NONE',  ( 30.87761267810551757, -2.376991648450896388, -225.4116222034606949 ) ) ;
#19478 = CARTESIAN_POINT ( 'NONE',  ( 14.61121792518381390, 23.81825453963186590, -227.9329146581663110 ) ) ;
#19479 = CARTESIAN_POINT ( 'NONE',  ( -14.94640692938030746, 5.382918922058764544, -220.5478552936960455 ) ) ;
#19480 = AXIS2_PLACEMENT_3D ( 'NONE', #12484, #3800, #9218 ) ;
#19481 = CARTESIAN_POINT ( 'NONE',  ( 16.00819137755116373, 4.595691552992191120, -229.5669508871464757 ) ) ;
#19482 = CARTESIAN_POINT ( 'NONE',  ( -18.40842514464981861, -18.33793064768350334, -230.6214457472987931 ) ) ;
#19483 = APPLICATION_CONTEXT ( 'automotive_design' ) ;
#19484 = CARTESIAN_POINT ( 'NONE',  ( 28.41961022423218353, 10.76616830294286409, -220.2698681100053193 ) ) ;
#19485 = CARTESIAN_POINT ( 'NONE',  ( -21.59049550158629316, -10.60627468734379164, -215.2236992441505663 ) ) ;
#19486 = CARTESIAN_POINT ( 'NONE',  ( -0.3197916200495275474, 16.38897215927557482, -229.9606066735827028 ) ) ;
#19487 = ADVANCED_FACE ( 'NONE', ( #6985 ), #13857, .F. ) ;
#19488 = AXIS2_PLACEMENT_3D ( 'NONE', #11436, #1079, #9862 ) ;
#19489 = CARTESIAN_POINT ( 'NONE',  ( 23.44028133050380802, 19.87677100428751231, -223.1503774981096342 ) ) ;
#19490 = AXIS2_PLACEMENT_3D ( 'NONE', #18246, #9688, #9359 ) ;
#19491 = CARTESIAN_POINT ( 'NONE',  ( -12.14452111807825041, 26.21581784948545035, -221.1455569020914140 ) ) ;
#19492 = CARTESIAN_POINT ( 'NONE',  ( -5.191169535941942748, 31.49570301054888688, -227.4714364261087098 ) ) ;
#19493 = CARTESIAN_POINT ( 'NONE',  ( 15.90795275983908574, 2.546196724714939297, -229.0855319561646297 ) ) ;
#19494 = CARTESIAN_POINT ( 'NONE',  ( 10.22171596740309418, -15.66339630224980972, -229.7686180632486810 ) ) ;
#19495 = CARTESIAN_POINT ( 'NONE',  ( 18.70674991763376482, -20.04093309878971496, -230.8534322170362714 ) ) ;
#19496 = LINE ( 'NONE', #11072, #14557 ) ;
#19497 = CARTESIAN_POINT ( 'NONE',  ( 16.64225601860865211, 1.926018578292457928, -220.2177910260893725 ) ) ;
#19498 = CARTESIAN_POINT ( 'NONE',  ( -29.78324924674133456, -0.2661018803894699136, -229.0431670511964057 ) ) ;
#19499 = CARTESIAN_POINT ( 'NONE',  ( -16.21268175593173311, -5.852138355245464219, -231.1837890105803410 ) ) ;
#19500 = CARTESIAN_POINT ( 'NONE',  ( 2.178520447619924472, -13.56847537563065487, -221.4085897031499428 ) ) ;
#19501 = CARTESIAN_POINT ( 'NONE',  ( 6.225744896574323839, 14.38227537199079720, -224.8391693295998266 ) ) ;
#19502 = DIRECTION ( 'NONE',  ( 1.000000000000000000, 0.000000000000000000, 0.000000000000000000 ) ) ;
#19503 = CARTESIAN_POINT ( 'NONE',  ( -11.84805200323110164, 5.835720598137266180, -228.2740675967047537 ) ) ;
#19504 = CARTESIAN_POINT ( 'NONE',  ( -6.101488798441174310, 11.33371047077072369, -225.3616985956418546 ) ) ;
#19505 = CARTESIAN_POINT ( 'NONE',  ( -3.139695637132168038, 25.12735071829084177, -230.1469660918596389 ) ) ;
#19506 = CARTESIAN_POINT ( 'NONE',  ( 16.37256825621668099, -5.086412116083368851, -216.7246661941694867 ) ) ;
#19507 = VERTEX_POINT ( 'NONE', #770 ) ;
#19508 = CONICAL_SURFACE ( 'NONE', #18814, 23.03038449397558196, 0.1745329251994333364 ) ;
#19509 = AXIS2_PLACEMENT_3D ( 'NONE', #4091, #2181, #9062 ) ;
#19510 = CARTESIAN_POINT ( 'NONE',  ( 15.26539804565921621, 9.309431686815628382, -232.9129599938668207 ) ) ;
#19511 = CARTESIAN_POINT ( 'NONE',  ( -22.53796032816233463, 16.84148256071415872, -226.0516062466300582 ) ) ;
#19512 = CARTESIAN_POINT ( 'NONE',  ( 22.49659352743751128, 7.060662713609715979, -215.7089950799439180 ) ) ;
#19513 = CARTESIAN_POINT ( 'NONE',  ( 1.250172743705837641, -19.35180105203422940, -231.6553945523530729 ) ) ;
#19514 = DIRECTION ( 'NONE',  ( 0.000000000000000000, 0.000000000000000000, 1.000000000000000000 ) ) ;
#19515 = DIRECTION ( 'NONE',  ( 0.000000000000000000, 0.000000000000000000, -1.000000000000000000 ) ) ;
#19516 = EDGE_CURVE ( 'NONE', #17512, #18185, #16094, .T. ) ;
#19517 = CARTESIAN_POINT ( 'NONE',  ( 11.33210854356620523, 22.81476816607802149, -217.8536224460118262 ) ) ;
#19518 = CARTESIAN_POINT ( 'NONE',  ( -31.13345889576667247, -1.683779982087686422, -229.5421043233184264 ) ) ;
#19519 = CARTESIAN_POINT ( 'NONE',  ( -15.83178333309709629, 2.467763724635483324, -230.4064772870105458 ) ) ;
#19520 = CARTESIAN_POINT ( 'NONE',  ( 13.99926435381047618, -21.11851526759364006, -232.9234173943665951 ) ) ;
#19521 = SHAPE_DEFINITION_REPRESENTATION ( #8534, #21505 ) ;
#19522 = CARTESIAN_POINT ( 'NONE',  ( 0.6364901924797052857, 13.89978473517355617, -221.8840706290426397 ) ) ;
#19524 = CARTESIAN_POINT ( 'NONE',  ( -18.41237742040652847, 14.06446039901721790, -216.7469276929859632 ) ) ;
#19523 = VECTOR ( 'NONE', #15287, 1000.000000000000000 ) ;
#19525 = CARTESIAN_POINT ( 'NONE',  ( -11.67631226053870996, 6.737291529340801333, -227.3110382950315227 ) ) ;
#19526 = CARTESIAN_POINT ( 'NONE',  ( -8.011291865669539547, -12.94570094964118923, -221.6322823144945744 ) ) ;
#19527 = VECTOR ( 'NONE', #5025, 1000.000000000000000 ) ;
#19528 = CARTESIAN_POINT ( 'NONE',  ( 0.000000000000000000, 0.000000000000000000, -60.00000000000000000 ) ) ;
#19529 = LINE ( 'NONE', #4115, #14541 ) ;
#19530 = CARTESIAN_POINT ( 'NONE',  ( -9.517741096562200909, 20.63709896626785678, -234.1036702156204967 ) ) ;
#19531 = CARTESIAN_POINT ( 'NONE',  ( 9.903783394593444811, -26.64562852513063973, -229.6560785209296682 ) ) ;
#19532 = CARTESIAN_POINT ( 'NONE',  ( -10.30050448363967419, 10.07750059423401190, -220.1837019037183723 ) ) ;
#19533 = CARTESIAN_POINT ( 'NONE',  ( -14.37318171526297483, 2.227741863946853140, -231.7654527934561202 ) ) ;
#19534 = CARTESIAN_POINT ( 'NONE',  ( 2.914696262605396715, 19.49933023975583879, -231.6035545612375017 ) ) ;
#19535 = LINE ( 'NONE', #20890, #13050 ) ;
#19536 = CARTESIAN_POINT ( 'NONE',  ( 16.55609572527610851, 2.729108819536508967, -230.5704679660131831 ) ) ;
#19537 = CARTESIAN_POINT ( 'NONE',  ( -16.95213199947759009, -16.93177456301608785, -219.4409135693619817 ) ) ;
#19538 = ORIENTED_EDGE ( 'NONE', *, *, #19894, .F. ) ;
#19539 = CARTESIAN_POINT ( 'NONE',  ( 8.674175678922351196, 20.85307874897338110, -216.6688793998777101 ) ) ;
#19540 = CARTESIAN_POINT ( 'NONE',  ( -11.10144104376680652, 18.49675466419975578, -232.2931259015917647 ) ) ;
#19541 = CARTESIAN_POINT ( 'NONE',  ( -8.137644474477026435, 12.10064032984799098, -226.6735072060122036 ) ) ;
#19542 = CARTESIAN_POINT ( 'NONE',  ( -12.38412712796990434, -11.70129718676926878, -221.8135637406489025 ) ) ;
#19543 = DIRECTION ( 'NONE',  ( -2.891205793294678696E-17, 0.000000000000000000, -1.000000000000000000 ) ) ;
#19544 = VERTEX_POINT ( 'NONE', #9234 ) ;
#19545 = CARTESIAN_POINT ( 'NONE',  ( -16.74550766701807447, 3.787526820511904813, -217.9802846976114381 ) ) ;
#19546 = CARTESIAN_POINT ( 'NONE',  ( 3.940243381406264511, -15.52098910442465041, -222.4744391328516144 ) ) ;
#19547 = CARTESIAN_POINT ( 'NONE',  ( 21.35706335192880445, 15.67286272432725092, -219.2578158352350783 ) ) ;
#19548 = CIRCLE ( 'NONE', #9855, 21.63401512838757768 ) ;
#19549 = CARTESIAN_POINT ( 'NONE',  ( 2.539761864897490007, 23.64215977235053501, -233.4645566207487661 ) ) ;
#19550 = UNCERTAINTY_MEASURE_WITH_UNIT (LENGTH_MEASURE( 1.000000000000000082E-05 ), #7619, 'distance_accuracy_value', 'NONE');
#19551 = CARTESIAN_POINT ( 'NONE',  ( -16.75232826114664775, 4.232868982398014346, -229.4158550594996200 ) ) ;
#19552 = EDGE_CURVE ( 'NONE', #18785, #17015, #19838, .T. ) ;
#19553 = CARTESIAN_POINT ( 'NONE',  ( 12.03015173539790617, 23.46358517874481109, -216.0611092640310744 ) ) ;
#19554 = CARTESIAN_POINT ( 'NONE',  ( 13.61707622192329481, 14.84143455326118932, -217.6958999636067063 ) ) ;
#19555 = CARTESIAN_POINT ( 'NONE',  ( 0.000000000000000000, 23.00000000000006040, 75.00000000000000000 ) ) ;
#19556 = CARTESIAN_POINT ( 'NONE',  ( -11.88525712185471050, -8.925198460467992589, -221.0951487055306472 ) ) ;
#19557 = CARTESIAN_POINT ( 'NONE',  ( 9.584731462935641488, -12.36622837314704348, -230.4796538097028531 ) ) ;
#19558 = DIRECTION ( 'NONE',  ( 0.000000000000000000, 1.000000000000000000, 0.000000000000000000 ) ) ;
#19559 = CIRCLE ( 'NONE', #21708, 19.80000000000007887 ) ;
#19560 = CARTESIAN_POINT ( 'NONE',  ( 0.000000000000000000, 22.63401512838754570, -77.51594804401857175 ) ) ;
#19561 = CARTESIAN_POINT ( 'NONE',  ( -10.14083745617744547, 19.87482866967577877, -216.0596634563153486 ) ) ;
#19562 = CARTESIAN_POINT ( 'NONE',  ( 11.78812147976811175, -1.482036947660514636, -224.5790252820172270 ) ) ;
#19563 = CARTESIAN_POINT ( 'NONE',  ( 27.36047156164216787, -8.591464759722228450, -221.3690063136810977 ) ) ;
#19564 = CARTESIAN_POINT ( 'NONE',  ( 12.98364502352995942, 13.67380631913144029, -233.1535077318696096 ) ) ;
#19565 = CARTESIAN_POINT ( 'NONE',  ( 8.132753622789847370, 14.44084924206385701, -222.7013822740049704 ) ) ;
#19566 = ORIENTED_EDGE ( 'NONE', *, *, #1509, .T. ) ;
#19567 = CARTESIAN_POINT ( 'NONE',  ( 6.114261689233397412, -11.26162238963769369, -223.0577857700231164 ) ) ;
#19568 = CARTESIAN_POINT ( 'NONE',  ( 15.76910524310159900, 5.601482066865847820, -220.3440822020379528 ) ) ;
#19569 = CARTESIAN_POINT ( 'NONE',  ( -4.619644865335168049, 14.75104250038670450, -232.3086264397671812 ) ) ;
#19570 = CARTESIAN_POINT ( 'NONE',  ( -10.30034651166687887, 25.05454868506992838, -216.5587736482213188 ) ) ;
#19571 = CARTESIAN_POINT ( 'NONE',  ( -30.71739798481564421, -2.702902032605977389, -225.9472362185736642 ) ) ;
#19572 = CARTESIAN_POINT ( 'NONE',  ( -15.82069055112642353, 8.315535108674763976, -217.2800172218543935 ) ) ;
#19573 = DIRECTION ( 'NONE',  ( -1.000000000000000000, 0.000000000000000000, 0.000000000000000000 ) ) ;
#19574 = CARTESIAN_POINT ( 'NONE',  ( 26.16486877413895584, -0.2437668799822691745, -230.8325409000573814 ) ) ;
#19575 = AXIS2_PLACEMENT_3D ( 'NONE', #18329, #7978, #2563 ) ;
#19576 = CARTESIAN_POINT ( 'NONE',  ( -0.7286890422672397394, 21.00519367000705273, -234.2149015821977969 ) ) ;
#19577 = CARTESIAN_POINT ( 'NONE',  ( 29.21307215008108216, 4.139194015751272104, -229.9658791484231699 ) ) ;
#19578 = CARTESIAN_POINT ( 'NONE',  ( -18.70100282803782576, 16.58357028540773115, -216.4425743468854080 ) ) ;
#19579 = CARTESIAN_POINT ( 'NONE',  ( 7.639528166734322667, 11.92751229241157596, -224.6077814063189635 ) ) ;
#19580 = DIRECTION ( 'NONE',  ( -2.162300680179986877E-16, -1.000000000000000000, 0.000000000000000000 ) ) ;
#19581 = VERTEX_POINT ( 'NONE', #7650 ) ;
#19582 = CARTESIAN_POINT ( 'NONE',  ( -2.117958212721558375, 27.20243410318316535, -230.7086725634165418 ) ) ;
#19583 = CARTESIAN_POINT ( 'NONE',  ( -13.52935284690462758, -5.503084506376929141, -222.3607690796775671 ) ) ;
#19584 = CARTESIAN_POINT ( 'NONE',  ( 9.333020543840051531, 16.91085096921651143, -217.7308990335875762 ) ) ;
#19585 = CARTESIAN_POINT ( 'NONE',  ( 10.30964016151751750, -15.48526446506176413, -234.8200832677974859 ) ) ;
#19586 = CARTESIAN_POINT ( 'NONE',  ( 20.79630060232323174, 1.171431775223809035, -222.2327692698370356 ) ) ;
#19587 = CARTESIAN_POINT ( 'NONE',  ( -21.19360951076126653, 12.15251088906093457, -217.9482185194656552 ) ) ;
#19588 = LINE ( 'NONE', #17481, #7414 ) ;
#19589 = CARTESIAN_POINT ( 'NONE',  ( 28.81324478616323148, -9.895151559995404966, -227.1624192579662918 ) ) ;
#19590 = EDGE_CURVE ( 'NONE', #9712, #15083, #4386, .T. ) ;
#19591 = CARTESIAN_POINT ( 'NONE',  ( 8.632180352507942800, 16.83956698119041917, -230.4752415867875186 ) ) ;
#19592 = CARTESIAN_POINT ( 'NONE',  ( -13.70798801564395752, 13.71024986321384809, -218.3360451569033955 ) ) ;
#19593 = CARTESIAN_POINT ( 'NONE',  ( -11.79271689233719478, 3.876813423829604144, -228.6816298097564299 ) ) ;
#19594 = CARTESIAN_POINT ( 'NONE',  ( -20.64589292112740537, -18.79971917946562598, -222.0410088502282520 ) ) ;
#19595 = CIRCLE ( 'NONE', #5541, 4.100000000000000533 ) ;
#19596 = AXIS2_PLACEMENT_3D ( 'NONE', #3617, #20386, #32 ) ;
#19597 = CARTESIAN_POINT ( 'NONE',  ( 22.66015888791822519, 10.43487984001084534, -234.3950629709119937 ) ) ;
#19598 = DIRECTION ( 'NONE',  ( -0.000000000000000000, -0.000000000000000000, 1.000000000000000000 ) ) ;
#19599 = CARTESIAN_POINT ( 'NONE',  ( -17.20514689733751368, -7.568958929800959190, -215.6459182133127115 ) ) ;
#19600 = CARTESIAN_POINT ( 'NONE',  ( -4.583529401292260275, 28.77615850237956607, -226.7744741901706504 ) ) ;
#19601 = CARTESIAN_POINT ( 'NONE',  ( 15.51129552754472307, 0.2180314803830030457, -231.3815478022924879 ) ) ;
#19602 = CARTESIAN_POINT ( 'NONE',  ( -10.24168223636446662, 16.14271751156598356, -231.4847994864913971 ) ) ;
#19603 = CARTESIAN_POINT ( 'NONE',  ( 12.90536070039565963, 17.66816134723717724, -234.8562535614228750 ) ) ;
#19604 = AXIS2_PLACEMENT_3D ( 'NONE', #247, #10268, #3830 ) ;
#19605 = CARTESIAN_POINT ( 'NONE',  ( -16.15126510923403202, -0.4755054218165427615, -219.3066569788202571 ) ) ;
#19606 = CARTESIAN_POINT ( 'NONE',  ( -3.496415903701482808, -16.44974864882642152, -218.6042005240371111 ) ) ;
#19607 =( GEOMETRIC_REPRESENTATION_CONTEXT ( 3 ) GLOBAL_UNCERTAINTY_ASSIGNED_CONTEXT ( ( #13029 ) ) GLOBAL_UNIT_ASSIGNED_CONTEXT ( ( #16011, #9262, #3844 ) ) REPRESENTATION_CONTEXT ( 'NONE', 'WORKASPACE' ) );
#19608 = CARTESIAN_POINT ( 'NONE',  ( 0.2799207934783670693, -28.72270877262613453, -227.3216717588132667 ) ) ;
#19609 = CARTESIAN_POINT ( 'NONE',  ( 0.000000000000000000, 23.00000000000006040, -60.00000000000000000 ) ) ;
#19610 = CARTESIAN_POINT ( 'NONE',  ( 20.23125423326388628, 7.836699765464857137, -217.8891354894872450 ) ) ;
#19611 = CARTESIAN_POINT ( 'NONE',  ( 11.39114332821395692, -8.257479203742953189, -226.5648397932267528 ) ) ;
#19612 = CARTESIAN_POINT ( 'NONE',  ( -21.63546480557098306, -21.44004028177477750, -223.8762611443524122 ) ) ;
#19613 = CARTESIAN_POINT ( 'NONE',  ( -13.13432812001650341, -19.42279346457301514, -216.4126494286626610 ) ) ;
#19614 = CARTESIAN_POINT ( 'NONE',  ( 9.489894741926459432, 25.96007012349547338, -222.3210984495278524 ) ) ;
#19615 = CARTESIAN_POINT ( 'NONE',  ( -21.80000000000000071, 0.000000000000000000, -78.50000000000000000 ) ) ;
#19616 = CARTESIAN_POINT ( 'NONE',  ( -13.84508897751235246, 5.904954704487344941, -218.7722818424232401 ) ) ;
#19617 = CARTESIAN_POINT ( 'NONE',  ( -9.151299407007059017, 9.196974979111923076, -223.9483834032048719 ) ) ;
#19618 = CARTESIAN_POINT ( 'NONE',  ( -1.364406401035816785, 24.33111505239456918, -219.5658712396381418 ) ) ;
#19619 = CARTESIAN_POINT ( 'NONE',  ( 13.95236037140391261, -4.360547358326352096, -218.9684814425422132 ) ) ;
#19620 = ORIENTED_EDGE ( 'NONE', *, *, #14219, .T. ) ;
#19621 = CARTESIAN_POINT ( 'NONE',  ( 23.18902850759750933, 20.27908137164207147, -226.2847847834817117 ) ) ;
#19622 = CARTESIAN_POINT ( 'NONE',  ( -21.10507617219916199, 14.90539259013048756, -229.7677326419877488 ) ) ;
#19623 = CARTESIAN_POINT ( 'NONE',  ( 27.79290571682592770, 12.05347838982552666, -230.1298045326732051 ) ) ;
#19624 = CARTESIAN_POINT ( 'NONE',  ( -0.8337089444836248697, -27.22572500676309559, -220.1932236949194532 ) ) ;
#19626 = DIRECTION ( 'NONE',  ( 1.000000000000000000, 6.982962677686272233E-15, 0.000000000000000000 ) ) ;
#19625 = AXIS2_PLACEMENT_3D ( 'NONE', #10884, #748, #19210 ) ;
#19627 = FACE_OUTER_BOUND ( 'NONE', #8030, .T. ) ;
#19628 = CARTESIAN_POINT ( 'NONE',  ( 18.29617186523616468, 23.20920553663278341, -223.4372550713720216 ) ) ;
#19629 = CARTESIAN_POINT ( 'NONE',  ( 20.43533161254376296, -19.75510188685668567, -224.2614117135439074 ) ) ;
#19630 = DIRECTION ( 'NONE',  ( -1.000000000000000000, -0.000000000000000000, -0.000000000000000000 ) ) ;
#19631 = CARTESIAN_POINT ( 'NONE',  ( -14.84823930505322132, -23.35465403802561823, -218.3226235040776260 ) ) ;
#19632 = CARTESIAN_POINT ( 'NONE',  ( 1.382955251742491898, 16.46353944795171032, -231.7743150979565030 ) ) ;
#19633 = CARTESIAN_POINT ( 'NONE',  ( -5.340143745732740754, 22.10628181454592678, -235.0476201740528097 ) ) ;
#19634 = ORIENTED_EDGE ( 'NONE', *, *, #5897, .T. ) ;
#19635 = CARTESIAN_POINT ( 'NONE',  ( -13.56774755469388616, 7.311522441667196226, -219.1912666243428021 ) ) ;
#19636 = CARTESIAN_POINT ( 'NONE',  ( -24.65069530437947876, -0.7989515219415058711, -216.4419420286324112 ) ) ;
#19637 = FACE_OUTER_BOUND ( 'NONE', #8352, .T. ) ;
#19638 = CARTESIAN_POINT ( 'NONE',  ( 0.000000000000000000, 0.000000000000000000, -65.00000000000000000 ) ) ;
#19639 = CARTESIAN_POINT ( 'NONE',  ( -9.540790481621398200, 9.981116473660406996, -228.6478862620407995 ) ) ;
#19640 = CARTESIAN_POINT ( 'NONE',  ( 8.072455080350884771, -13.51419333260225741, -221.0758372092125228 ) ) ;
#19641 = PRESENTATION_STYLE_ASSIGNMENT (( #12795 ) ) ;
#19642 = CARTESIAN_POINT ( 'NONE',  ( -12.90983082593748676, 14.84936372681532823, -233.8009687022269532 ) ) ;
#19643 = CARTESIAN_POINT ( 'NONE',  ( 18.39384604806649648, 2.566915855367216004, -231.7421336352533103 ) ) ;
#19644 = CARTESIAN_POINT ( 'NONE',  ( -8.328662059352005542, 28.53523473722178139, -221.4280032538016201 ) ) ;
#19645 = LINE ( 'NONE', #858, #107 ) ;
#19646 = CARTESIAN_POINT ( 'NONE',  ( 17.92683513449900445, 4.153309877386362814, -218.0960491240478234 ) ) ;
#19647 = CARTESIAN_POINT ( 'NONE',  ( -10.06242375715308945, -19.11710762076843295, -231.0938065448402199 ) ) ;
#19648 = ORIENTED_EDGE ( 'NONE', *, *, #21825, .F. ) ;
#19649 = CARTESIAN_POINT ( 'NONE',  ( 12.95792863868717149, 16.83236386576623644, -216.3406066345214356 ) ) ;
#19650 = CARTESIAN_POINT ( 'NONE',  ( -10.45265333418718612, 16.71118685480038479, -231.7490466715443631 ) ) ;
#19651 = CARTESIAN_POINT ( 'NONE',  ( -9.746008880186941781, 12.96562886885531896, -220.1990846131056401 ) ) ;
#19652 = CARTESIAN_POINT ( 'NONE',  ( 27.54201077264015396, -3.286392687948289648, -218.1575117614944190 ) ) ;
#19653 = CARTESIAN_POINT ( 'NONE',  ( 12.50000000000000355, 0.000000000000000000, -25.00000000000000000 ) ) ;
#19654 = ORIENTED_EDGE ( 'NONE', *, *, #7567, .F. ) ;
#19655 = CARTESIAN_POINT ( 'NONE',  ( -29.95012366401462955, 4.746560250930182967, -224.6954343660969471 ) ) ;
#19656 = CARTESIAN_POINT ( 'NONE',  ( -4.451292041429703694, -15.86428280493796628, -231.0943874731633798 ) ) ;
#19657 = CARTESIAN_POINT ( 'NONE',  ( 14.66712853512338732, 1.689060028942728442, -227.4794820723986390 ) ) ;
#19658 = CARTESIAN_POINT ( 'NONE',  ( -2.735889804569492600, 12.71735652435744512, -225.1194195722198117 ) ) ;
#19659 = CARTESIAN_POINT ( 'NONE',  ( 1.317067778529001989E-13, -19.63401512838754215, 77.51594804401857175 ) ) ;
#19660 = CARTESIAN_POINT ( 'NONE',  ( 21.75737151495493649, -2.205713500382455283, -233.2756072794337285 ) ) ;
#19661 = CARTESIAN_POINT ( 'NONE',  ( 15.23494377589453919, 15.24947835004434538, -215.7641128510430519 ) ) ;
#19662 = CARTESIAN_POINT ( 'NONE',  ( 22.46220731426537043, 18.23201731183003460, -227.5436199598787539 ) ) ;
#19663 = CARTESIAN_POINT ( 'NONE',  ( -12.50000000000000000, 0.000000000000000000, 94.00000000000000000 ) ) ;
#19664 = CARTESIAN_POINT ( 'NONE',  ( -27.99742768613627319, -7.906662303124995184, -217.4094589651611216 ) ) ;
#19665 = CARTESIAN_POINT ( 'NONE',  ( -5.519971913460887336, -12.21762732219001713, -227.2962593638428359 ) ) ;
#19666 = CARTESIAN_POINT ( 'NONE',  ( 14.99336262864975211, -23.54026314425397004, -231.3018640253376361 ) ) ;
#19667 = CARTESIAN_POINT ( 'NONE',  ( -22.97082590106532507, -1.326754249648130157, -9.933407853828526868 ) ) ;
#19668 = CARTESIAN_POINT ( 'NONE',  ( 1.665334536937735820E-13, -23.00000000000006040, -69.99999999999998579 ) ) ;
#19669 = CARTESIAN_POINT ( 'NONE',  ( -4.211886032913159106, 20.62037006687756602, -216.9488349035050305 ) ) ;
#19670 = CARTESIAN_POINT ( 'NONE',  ( 30.80938026993025503, 0.02210899415489638725, -229.5596456628577187 ) ) ;
#19671 = CARTESIAN_POINT ( 'NONE',  ( 14.02668320743028119, -5.282748560960272677, -221.9001732195871739 ) ) ;
#19672 = CARTESIAN_POINT ( 'NONE',  ( -20.97727766418175932, 9.381545086430262970, -232.5968905491617420 ) ) ;
#19673 = CARTESIAN_POINT ( 'NONE',  ( 21.26803326031697949, 19.54255073453192892, -230.5813148908474659 ) ) ;
#19674 = CARTESIAN_POINT ( 'NONE',  ( 12.16813927252146144, 18.27141895336136912, -230.9123895730235745 ) ) ;
#19675 = VERTEX_POINT ( 'NONE', #4255 ) ;
#19676 = CARTESIAN_POINT ( 'NONE',  ( 4.354371064427007276, -19.91633591276652382, -233.4790676556106348 ) ) ;
#19677 = CARTESIAN_POINT ( 'NONE',  ( 16.07305932912010960, 0.9253679043337685872, -229.0409936706996064 ) ) ;
#19678 = ADVANCED_FACE ( 'NONE', ( #11027 ), #17894, .T. ) ;
#19679 = CARTESIAN_POINT ( 'NONE',  ( -7.403072389817287657, 18.92851032520892929, -215.2068968469505137 ) ) ;
#19680 = CARTESIAN_POINT ( 'NONE',  ( -7.752954785937490989, 10.21341112307795385, -225.5135920495299615 ) ) ;
#19681 = CARTESIAN_POINT ( 'NONE',  ( -28.57583275380518018, -9.842401781236429059, -222.4643230566485386 ) ) ;
#19682 = CARTESIAN_POINT ( 'NONE',  ( -9.716674560061926869, 27.56227806819028103, -219.4917914922789919 ) ) ;
#19683 = CARTESIAN_POINT ( 'NONE',  ( -20.26851768784797869, -0.8260594303982465858, -217.1279713726092098 ) ) ;
#19684 = CARTESIAN_POINT ( 'NONE',  ( 17.00614511541963836, -1.958782916976874233, -219.4638360731791806 ) ) ;
#19685 = CARTESIAN_POINT ( 'NONE',  ( -3.162425552858488143, 20.40327580806445695, -216.0004724541873316 ) ) ;
#19686 = CARTESIAN_POINT ( 'NONE',  ( 27.79290571682592770, 12.05347838982552666, -230.1298045326732051 ) ) ;
#19687 = CARTESIAN_POINT ( 'NONE',  ( -25.61997837663875188, 10.01664178086244483, -231.6711741719404074 ) ) ;
#19688 = CARTESIAN_POINT ( 'NONE',  ( 12.71450444683213021, 7.595266944807587350, -224.4213778964231665 ) ) ;
#19689 = CARTESIAN_POINT ( 'NONE',  ( 1.232595164407830946E-29, -17.50000000000007105, -24.99999999999999645 ) ) ;
#19690 = CARTESIAN_POINT ( 'NONE',  ( 0.07890756785233743464, 25.14108539708653822, -218.4152285319504756 ) ) ;
#19691 = CARTESIAN_POINT ( 'NONE',  ( -25.98129645912436914, -15.13773040547512139, -224.1390156429105787 ) ) ;
#19692 = CARTESIAN_POINT ( 'NONE',  ( 21.25094435758043332, 17.68230636442804027, -229.7964888993842010 ) ) ;
#19693 = CARTESIAN_POINT ( 'NONE',  ( -0.8305687497496098137, -27.95880702065288759, -232.3543905114424888 ) ) ;
#19694 = CARTESIAN_POINT ( 'NONE',  ( 18.77038210872052559, 2.992569296362963538, -224.7568172542696914 ) ) ;
#19695 = CARTESIAN_POINT ( 'NONE',  ( -14.24491355791863612, 5.286533920242113105, -221.7104936369346433 ) ) ;
#19696 = CARTESIAN_POINT ( 'NONE',  ( 18.03651828442428595, -19.10816016050398147, -231.7458924702002037 ) ) ;
#19697 = CARTESIAN_POINT ( 'NONE',  ( 8.829458998963966465, 22.90677303676718779, -219.2026791561175685 ) ) ;
#19698 = CARTESIAN_POINT ( 'NONE',  ( -24.18895665211001500, 11.26087434487096139, -231.0040666710689550 ) ) ;
#19700 = AXIS2_PLACEMENT_3D ( 'NONE', #19951, #12777, #7715 ) ;
#19699 = CARTESIAN_POINT ( 'NONE',  ( -26.12939716039095117, 11.33146045174629357, -233.1192402782019997 ) ) ;
#19701 = CARTESIAN_POINT ( 'NONE',  ( -9.481788909210624894, -22.96916533494018253, -217.3969400264330716 ) ) ;
#19702 = EDGE_CURVE ( 'NONE', #14415, #12893, #21356, .T. ) ;
#19703 = CARTESIAN_POINT ( 'NONE',  ( 13.40064012097826307, 2.532414129335418096, -221.5952957478750989 ) ) ;
#19704 = FACE_OUTER_BOUND ( 'NONE', #10631, .T. ) ;
#19705 = CARTESIAN_POINT ( 'NONE',  ( -11.65988442122670676, -3.998659314375652141, -223.4258670541443621 ) ) ;
#19706 = CARTESIAN_POINT ( 'NONE',  ( 2.579827969572558111, 15.91317371615649101, -219.7652087782269916 ) ) ;
#19707 = CARTESIAN_POINT ( 'NONE',  ( 20.13946171159960841, -0.1427001808266660232, -233.7987036390019853 ) ) ;
#19708 = CARTESIAN_POINT ( 'NONE',  ( -5.590964611773372894, 13.92546790642523113, -228.7941110425196882 ) ) ;
#19709 = EDGE_CURVE ( 'NONE', #9941, #10887, #16281, .T. ) ;
#19710 = AXIS2_PLACEMENT_3D ( 'NONE', #4131, #7961, #4455 ) ;
#19711 = CARTESIAN_POINT ( 'NONE',  ( 12.58577552758108986, 11.40439409249366420, -217.4478085440898951 ) ) ;
#19712 = CARTESIAN_POINT ( 'NONE',  ( 3.050495372378628112, -23.18092737088175781, -231.5841725462776992 ) ) ;
#19713 = ORIENTED_EDGE ( 'NONE', *, *, #17601, .T. ) ;
#19714 = CARTESIAN_POINT ( 'NONE',  ( 6.755953262402430326, -28.44658494672641424, -224.7309905328439754 ) ) ;
#19715 = ADVANCED_FACE ( 'NONE', ( #16309 ), #14845, .T. ) ;
#19716 = CARTESIAN_POINT ( 'NONE',  ( 20.89184612657454920, 5.404957034965973683, -232.0952743654565609 ) ) ;
#19717 = CARTESIAN_POINT ( 'NONE',  ( 14.34945462593695531, -6.128426910066905542, -229.1128190117150041 ) ) ;
#19718 = EDGE_CURVE ( 'NONE', #8548, #7880, #14856, .T. ) ;
#19719 = CARTESIAN_POINT ( 'NONE',  ( 18.65267415280877117, -0.4843198157805662651, -217.0419311198673711 ) ) ;
#19720 = CARTESIAN_POINT ( 'NONE',  ( -10.42804209284631156, -14.08702332024887305, -217.7386024361820489 ) ) ;
#19721 = CARTESIAN_POINT ( 'NONE',  ( 3.635089269978064141, 27.05650967970794341, -222.4639105745756638 ) ) ;
#19722 =( NAMED_UNIT ( * ) SI_UNIT ( $, .STERADIAN. ) SOLID_ANGLE_UNIT ( ) );
#19723 = CARTESIAN_POINT ( 'NONE',  ( -22.28357709049062407, 7.264818440526320309, -215.3877468064711707 ) ) ;
#19724 = CARTESIAN_POINT ( 'NONE',  ( -0.3969026096611234511, 20.89748314411456676, -216.3289738411752978 ) ) ;
#19725 = CARTESIAN_POINT ( 'NONE',  ( 3.191455400233187412, 17.67480163422566619, -220.7055581859663107 ) ) ;
#19726 = CARTESIAN_POINT ( 'NONE',  ( -22.05223281125446633, 0.4748437386657422543, -217.8785187290425256 ) ) ;
#19727 = ORIENTED_EDGE ( 'NONE', *, *, #14990, .T. ) ;
#19728 = CARTESIAN_POINT ( 'NONE',  ( 18.81274554574540403, 10.85963742466947224, -234.0446454529665345 ) ) ;
#19729 = CARTESIAN_POINT ( 'NONE',  ( -22.36207348798144778, 17.12313795477538036, -223.8571857210765472 ) ) ;
#19730 = CARTESIAN_POINT ( 'NONE',  ( -22.14646582578067679, 6.967411055428133437, -231.6932229095398270 ) ) ;
#19731 = CARTESIAN_POINT ( 'NONE',  ( -5.249799428260828904, -14.16826377401270065, -226.9124264195330056 ) ) ;
#19732 = CYLINDRICAL_SURFACE ( 'NONE', #7971, 21.00000000000008171 ) ;
#19733 = DIRECTION ( 'NONE',  ( 0.000000000000000000, 0.6000000000000004219, 0.7999999999999997113 ) ) ;
#19734 = CARTESIAN_POINT ( 'NONE',  ( 4.656903975822286768, 13.45000048768594780, -227.6722060245555497 ) ) ;
#19735 = CARTESIAN_POINT ( 'NONE',  ( 17.22969587606878505, -8.834803756807117381, -230.2348533348707917 ) ) ;
#19736 = CARTESIAN_POINT ( 'NONE',  ( 14.83290459615719215, -2.296615622475745688, -226.9301701175285757 ) ) ;
#19737 = CARTESIAN_POINT ( 'NONE',  ( -7.349743644505656093, -15.31718010764164539, -232.4470764718129772 ) ) ;
#19738 = APPLICATION_PROTOCOL_DEFINITION ( 'draft international standard', 'automotive_design', 1998, #4528 ) ;
#19739 = CARTESIAN_POINT ( 'NONE',  ( -2.772442535524381579, 13.75675912271027457, -228.9770533867650215 ) ) ;
#19740 = CARTESIAN_POINT ( 'NONE',  ( -3.687581766460184429, 30.01855770642711718, -218.8323691868875187 ) ) ;
#19741 = VERTEX_POINT ( 'NONE', #7980 ) ;
#19742 = CARTESIAN_POINT ( 'NONE',  ( -12.44873260470819787, 7.411970124596155785, -229.4214091473984070 ) ) ;
#19743 = CARTESIAN_POINT ( 'NONE',  ( -25.32486352395475393, -3.505876693931964549, -233.0869506614649822 ) ) ;
#19744 = CARTESIAN_POINT ( 'NONE',  ( -22.91305488956320957, -9.999595782860119186, -0.6663400851647119927 ) ) ;
#19745 = DIRECTION ( 'NONE',  ( 0.000000000000000000, 0.000000000000000000, 1.000000000000000000 ) ) ;
#19746 = CARTESIAN_POINT ( 'NONE',  ( -11.69688825528096388, 18.63404371591177622, -215.8612738028812714 ) ) ;
#19747 = CARTESIAN_POINT ( 'NONE',  ( -6.773088999562194346, -28.54379939428971369, -218.3283227997898450 ) ) ;
#19748 = CARTESIAN_POINT ( 'NONE',  ( 14.34945462593695531, -6.128426910066905542, -229.1128190117150041 ) ) ;
#19749 = CARTESIAN_POINT ( 'NONE',  ( -9.740348021262962064, 16.12529029871877384, -216.4361617420699702 ) ) ;
#19750 = CARTESIAN_POINT ( 'NONE',  ( -12.10258892854866275, 5.599955477755926836, -221.6590149575334010 ) ) ;
#19751 = CARTESIAN_POINT ( 'NONE',  ( -2.117958212721558375, 27.20243410318316535, -230.7086725634165418 ) ) ;
#19752 = PLANE ( 'NONE',  #22016 ) ;
#19753 = CARTESIAN_POINT ( 'NONE',  ( 22.24262848503957812, 2.205713500382371794, -232.7243927205662430 ) ) ;
#19754 = CARTESIAN_POINT ( 'NONE',  ( -18.95931133506032040, -20.40484553783743138, -225.1835090426186525 ) ) ;
#19755 = ORIENTED_EDGE ( 'NONE', *, *, #15025, .T. ) ;
#19756 = CARTESIAN_POINT ( 'NONE',  ( 6.771176146757415637, 15.60014285904435027, -218.3493856697694753 ) ) ;
#19757 = CARTESIAN_POINT ( 'NONE',  ( -16.45414350258782221, 17.57852913985137988, -231.3969631806205598 ) ) ;
#19758 = CARTESIAN_POINT ( 'NONE',  ( -15.05930145804884290, 24.78193219970826533, -223.0510781988847953 ) ) ;
#19759 = CARTESIAN_POINT ( 'NONE',  ( -24.76242154467160717, -4.839146110080178254, -231.6857664014047202 ) ) ;
#19760 = DIRECTION ( 'NONE',  ( 0.000000000000000000, 0.000000000000000000, -1.000000000000000000 ) ) ;
#19761 = VERTEX_POINT ( 'NONE', #11355 ) ;
#19762 = CARTESIAN_POINT ( 'NONE',  ( 21.19180206786061405, -1.472355559550188264, -231.3901500139509722 ) ) ;
#19763 = CARTESIAN_POINT ( 'NONE',  ( -8.861553082841476581, -17.08180233781500590, -216.2529452235939402 ) ) ;
#19764 = CARTESIAN_POINT ( 'NONE',  ( 18.46552355142154411, 5.019711608606525211, -231.5099115070375433 ) ) ;
#19765 = CARTESIAN_POINT ( 'NONE',  ( 5.169766346882679997, 29.28517558595074988, -221.5178724947562614 ) ) ;
#19766 = DIRECTION ( 'NONE',  ( 0.000000000000000000, 0.000000000000000000, -1.000000000000000000 ) ) ;
#19767 = CARTESIAN_POINT ( 'NONE',  ( -17.91769793922991028, 3.277678596821882007, -219.5526088240203819 ) ) ;
#19768 = CARTESIAN_POINT ( 'NONE',  ( 10.46530733675539793, 8.351728317179080818, -222.7431177495969621 ) ) ;
#19769 = PRESENTATION_STYLE_ASSIGNMENT (( #21795 ) ) ;
#19770 = CARTESIAN_POINT ( 'NONE',  ( -23.45461921731179800, 8.654954236178731719, -5.019855114128365159 ) ) ;
#19771 = CARTESIAN_POINT ( 'NONE',  ( 24.42567939027770407, 10.22651298688739097, -219.4562066833365748 ) ) ;
#19772 = CARTESIAN_POINT ( 'NONE',  ( -25.00000000000000000, -1.002884296170500229E-19, 10.00000000000000000 ) ) ;
#19773 = CARTESIAN_POINT ( 'NONE',  ( 25.75976839005050323, -3.608312289253767347, -220.3697909415571417 ) ) ;
#19774 = CARTESIAN_POINT ( 'NONE',  ( -27.88251101234890328, -7.575382714962081820, -221.6715981084135478 ) ) ;
#19775 = DIRECTION ( 'NONE',  ( 1.000000000000000000, 0.000000000000000000, 0.000000000000000000 ) ) ;
#19776 = DIRECTION ( 'NONE',  ( 1.000000000000000000, 0.000000000000000000, -0.000000000000000000 ) ) ;
#19777 = CARTESIAN_POINT ( 'NONE',  ( -1.946052076048385482, 22.23149728939677061, -232.8927760318659068 ) ) ;
#19778 = CARTESIAN_POINT ( 'NONE',  ( 29.48160760559006732, -8.328447718542550504, -230.7159994440206390 ) ) ;
#19779 = CARTESIAN_POINT ( 'NONE',  ( 19.06763123184207487, -2.048228142369658666, -218.2337357994572073 ) ) ;
#19780 = CARTESIAN_POINT ( 'NONE',  ( -15.36327147092456791, 5.453733681707060299, -220.0043800961136355 ) ) ;
#19781 = CARTESIAN_POINT ( 'NONE',  ( 17.24952650401854370, 25.19767938110938843, -224.5319471861414797 ) ) ;
#19782 = CARTESIAN_POINT ( 'NONE',  ( 14.78510113471881304, 14.77128235908076803, -230.8056908117964383 ) ) ;
#19783 = ORIENTED_EDGE ( 'NONE', *, *, #550, .F. ) ;
#19784 = CARTESIAN_POINT ( 'NONE',  ( 0.7148793108008648645, -17.78534256477599840, -218.6573294195452775 ) ) ;
#19785 = CARTESIAN_POINT ( 'NONE',  ( 4.401501667365108617, 18.53594119471695123, -215.1186850315663150 ) ) ;
#19786 = CARTESIAN_POINT ( 'NONE',  ( -10.33514150881494942, 13.62639309082336503, -216.9544063991933172 ) ) ;
#19787 = CARTESIAN_POINT ( 'NONE',  ( 28.44445586451508845, -4.662230540760189612, -220.9797193573593290 ) ) ;
#19788 = CARTESIAN_POINT ( 'NONE',  ( -3.855805549595750392, 26.68244055262801950, -232.4569730455296508 ) ) ;
#19789 = CARTESIAN_POINT ( 'NONE',  ( -10.34058050218014735, -10.16585704662449174, 93.00000000000000000 ) ) ;
#19790 = EDGE_CURVE ( 'NONE', #10050, #21036, #120, .T. ) ;
#19791 = CARTESIAN_POINT ( 'NONE',  ( -5.836418080594380164, 30.19240250712089590, -223.8354869487762357 ) ) ;
#19792 = CARTESIAN_POINT ( 'NONE',  ( 12.66989206167516357, 2.082990619159506007, -225.6419847029432901 ) ) ;
#19793 = CARTESIAN_POINT ( 'NONE',  ( -24.24202834850560606, 19.05981756344202438, -226.6980666352953335 ) ) ;
#19794 = CARTESIAN_POINT ( 'NONE',  ( 14.32085100525799248, 9.220655089380342062, -219.9006227404039464 ) ) ;
#19795 = CARTESIAN_POINT ( 'NONE',  ( 3.198229568054530070, 16.42319727383711481, -222.3960047798183552 ) ) ;
#19796 = CARTESIAN_POINT ( 'NONE',  ( 0.000000000000000000, 25.00000000000000000, 75.00000000000000000 ) ) ;
#19797 = CARTESIAN_POINT ( 'NONE',  ( -4.824452364631481416, 22.01523768541901305, -216.8350837474290245 ) ) ;
#19798 = CARTESIAN_POINT ( 'NONE',  ( -8.514447835183077018, -10.26590951297754195, -225.5321622820681569 ) ) ;
#19799 = CARTESIAN_POINT ( 'NONE',  ( 17.99029889091409018, 9.613712288440757092, -232.0298403238024036 ) ) ;
#19800 = CARTESIAN_POINT ( 'NONE',  ( -9.981957700435337699, -28.23530775694580441, -222.3321348641582347 ) ) ;
#19801 = CARTESIAN_POINT ( 'NONE',  ( 18.80464855560519055, 2.963306505625483922, -224.5168608946970323 ) ) ;
#19802 = CARTESIAN_POINT ( 'NONE',  ( -22.07068341299880743, 18.38202870573248049, -227.7785760498121306 ) ) ;
#19803 = LINE ( 'NONE', #17922, #2365 ) ;
#19804 = CARTESIAN_POINT ( 'NONE',  ( 8.339826811406878093, -13.81198187275966660, -229.8741491687588621 ) ) ;
#19805 = CARTESIAN_POINT ( 'NONE',  ( 7.042184411928968935, 23.28260216771182556, -230.5707103145148267 ) ) ;
#19806 = CARTESIAN_POINT ( 'NONE',  ( -10.16319438574952372, 11.71174522937666040, -227.8434026503654479 ) ) ;
#19807 = CARTESIAN_POINT ( 'NONE',  ( -30.17036082276531772, 5.959165309317525860, -219.4883053239162791 ) ) ;
#19808 = CARTESIAN_POINT ( 'NONE',  ( -16.80743794350546594, -8.145538706591455735, -220.2004866397506078 ) ) ;
#19809 = CARTESIAN_POINT ( 'NONE',  ( 14.29548763234129538, 2.320071712424730315, -230.2610858871018422 ) ) ;
#19810 = CIRCLE ( 'NONE', #6162, 23.00000000000000000 ) ;
#19811 = CARTESIAN_POINT ( 'NONE',  ( 17.50000000000000355, 0.000000000000000000, -65.00000000000000000 ) ) ;
#19812 = CARTESIAN_POINT ( 'NONE',  ( -10.37549270978917448, -7.969494006339708392, -220.1790165754723603 ) ) ;
#19813 = CARTESIAN_POINT ( 'NONE',  ( 2.485733319737138736, 14.76073968410796056, -221.5245536174130905 ) ) ;
#19814 = CARTESIAN_POINT ( 'NONE',  ( 12.88374853655145458, 4.106359831454843068, -228.1016120772327440 ) ) ;
#19815 = CIRCLE ( 'NONE', #2576, 23.00000000000000000 ) ;
#19816 = CARTESIAN_POINT ( 'NONE',  ( -16.48883219358909713, 20.84100960965193394, -219.4392138569792507 ) ) ;
#19817 = CARTESIAN_POINT ( 'NONE',  ( 10.82528077991200810, 8.849546035972329250, -221.2068619981234008 ) ) ;
#19818 = ADVANCED_FACE ( 'NONE', ( #9667 ), #10529, .T. ) ;
#19819 = CARTESIAN_POINT ( 'NONE',  ( 3.208289162541382300, -18.46136333555241293, -230.6641274008648850 ) ) ;
#19820 = CARTESIAN_POINT ( 'NONE',  ( -1.198425787605166715, -24.00698511249634137, -218.1862405767648170 ) ) ;
#19821 = AXIS2_PLACEMENT_3D ( 'NONE', #6630, #13500, #8657 ) ;
#19822 = CARTESIAN_POINT ( 'NONE',  ( 26.29894631880581812, 12.29609390142961090, -226.3100047295820332 ) ) ;
#19823 = CARTESIAN_POINT ( 'NONE',  ( 24.96294718070021901, -13.86220829677249178, -229.4442241490162075 ) ) ;
#19824 = CARTESIAN_POINT ( 'NONE',  ( -24.76115377241536208, -2.015397159694146456, -231.8500816169410825 ) ) ;
#19825 = CARTESIAN_POINT ( 'NONE',  ( -12.11864581566431553, -23.10742878804749978, -232.9192999331436909 ) ) ;
#19826 = CARTESIAN_POINT ( 'NONE',  ( 14.96080648943632241, 22.28365808184747721, -220.1237743409445216 ) ) ;
#19827 = CARTESIAN_POINT ( 'NONE',  ( -12.10258892854866275, 5.599955477755926836, -221.6590149575334010 ) ) ;
#19828 = CARTESIAN_POINT ( 'NONE',  ( 2.539761864897490007, 23.64215977235053501, -233.4645566207487661 ) ) ;
#19829 = CARTESIAN_POINT ( 'NONE',  ( -2.426309470044460959, 27.69042070294474556, -223.4541227565655674 ) ) ;
#19830 = CARTESIAN_POINT ( 'NONE',  ( 13.42973690470193837, -10.83953015014330035, -233.9990574442320224 ) ) ;
#19831 = CARTESIAN_POINT ( 'NONE',  ( 12.08198696763335178, 15.54678077493410981, -216.6084679670902631 ) ) ;
#19832 = CARTESIAN_POINT ( 'NONE',  ( -21.67128887413246119, 15.53484693247673043, -229.0088198863946900 ) ) ;
#19833 = CARTESIAN_POINT ( 'NONE',  ( -18.93763370444446181, -0.7340653299870684156, -219.7345063954518594 ) ) ;
#19834 = ADVANCED_FACE ( 'NONE', ( #21688 ), #11973, .T. ) ;
#19835 = CARTESIAN_POINT ( 'NONE',  ( 1.967796959512672306, -15.42100964229427085, -222.1538042820122314 ) ) ;
#19836 = CARTESIAN_POINT ( 'NONE',  ( 25.50000000000000000, 3.600000000000000533, -2.700000000000000622 ) ) ;
#19837 = DIRECTION ( 'NONE',  ( -1.000000000000000000, 0.000000000000000000, 0.000000000000000000 ) ) ;
#19838 = CIRCLE ( 'NONE', #17712, 2.000000000000000000 ) ;
#19839 = CARTESIAN_POINT ( 'NONE',  ( 25.33562512631297281, 12.25422971834577268, -228.6777356031426791 ) ) ;
#19840 = CARTESIAN_POINT ( 'NONE',  ( 12.71657619101469194, -13.18628128886902040, -219.4305778833985414 ) ) ;
#19841 = CARTESIAN_POINT ( 'NONE',  ( 26.00000000000000000, 1.360023205165816762E-13, 0.000000000000000000 ) ) ;
#19842 = CARTESIAN_POINT ( 'NONE',  ( -5.519971913460887336, -12.21762732219001713, -227.2962593638428359 ) ) ;
#19843 = APPLICATION_PROTOCOL_DEFINITION ( 'draft international standard', 'automotive_design', 1998, #14477 ) ;
#19844 = CARTESIAN_POINT ( 'NONE',  ( -2.208416658185406334, 29.10348627872611615, -219.8480645685746424 ) ) ;
#19845 = CARTESIAN_POINT ( 'NONE',  ( -1.584125552723561592, 20.48724127025963782, -214.7515060525244621 ) ) ;
#19846 = ORIENTED_EDGE ( 'NONE', *, *, #8856, .T. ) ;
#19847 = CARTESIAN_POINT ( 'NONE',  ( -16.65698539163286540, 11.03290537638306112, -233.6474915129378758 ) ) ;
#19848 = CARTESIAN_POINT ( 'NONE',  ( 27.38348740615853316, -3.050674415727137045, -231.0934891209028876 ) ) ;
#19849 = CARTESIAN_POINT ( 'NONE',  ( -23.84416809906481305, -7.516854498463030332, 6.603279950623392125 ) ) ;
#19850 = CARTESIAN_POINT ( 'NONE',  ( -21.58811430103374818, 7.943727580301767510, -6.108684005820687268 ) ) ;
#19851 = CARTESIAN_POINT ( 'NONE',  ( -12.74846050492543625, 19.93509882904884734, -216.0172840992881049 ) ) ;
#19852 = CARTESIAN_POINT ( 'NONE',  ( -3.265885032814331623, -11.59335615597398217, -224.1764024733101053 ) ) ;
#19853 = CIRCLE ( 'NONE', #15912, 23.00000000000008882 ) ;
#19854 = DIRECTION ( 'NONE',  ( 0.000000000000000000, 0.000000000000000000, -1.000000000000000000 ) ) ;
#19855 = CARTESIAN_POINT ( 'NONE',  ( -15.20262116893801974, 8.038155052917188570, -217.6767387945475036 ) ) ;
#19856 = AXIS2_PLACEMENT_3D ( 'NONE', #21293, #21190, #14023 ) ;
#19857 = CARTESIAN_POINT ( 'NONE',  ( 15.58465056415575312, 2.812367138262562349, -229.5090343034091234 ) ) ;
#19858 = CARTESIAN_POINT ( 'NONE',  ( 3.100794261777709782, 20.70580715608724276, -231.8781843337728219 ) ) ;
#19859 = CARTESIAN_POINT ( 'NONE',  ( 0.000000000000000000, 0.000000000000000000, 69.99999999999998579 ) ) ;
#19860 = CARTESIAN_POINT ( 'NONE',  ( 14.73597170006453361, 7.272367905564328439, -221.0092474305599239 ) ) ;
#19861 = CARTESIAN_POINT ( 'NONE',  ( -13.03991958801536555, -12.43893258430110471, -220.5791972147702040 ) ) ;
#19862 = ORIENTED_EDGE ( 'NONE', *, *, #5142, .F. ) ;
#19863 = CARTESIAN_POINT ( 'NONE',  ( -11.35482716595652875, 11.86850131893102223, -220.6599844941370350 ) ) ;
#19864 = CARTESIAN_POINT ( 'NONE',  ( 7.018811797190238622, 13.93862807232938472, -230.2855929063610176 ) ) ;
#19865 = CARTESIAN_POINT ( 'NONE',  ( -1.406618399933933006, 16.47239985789244443, -232.2564017133012726 ) ) ;
#19866 = EDGE_CURVE ( 'NONE', #3746, #15108, #11240, .T. ) ;
#19867 = VERTEX_POINT ( 'NONE', #18110 ) ;
#19868 = CARTESIAN_POINT ( 'NONE',  ( 29.37495210618232022, -3.074218464324032229, -220.1817713028459025 ) ) ;
#19869 = CARTESIAN_POINT ( 'NONE',  ( 2.999999999999971578, 3.673940397442062826E-16, -221.9999999999999716 ) ) ;
#19870 = ORIENTED_EDGE ( 'NONE', *, *, #6828, .F. ) ;
#19871 = CARTESIAN_POINT ( 'NONE',  ( -11.79584727357715934, 6.509288465425584036, -222.6080315736180921 ) ) ;
#19872 = CARTESIAN_POINT ( 'NONE',  ( -18.76818401764774080, -23.60322278862490109, -229.9112526505913365 ) ) ;
#19873 = CARTESIAN_POINT ( 'NONE',  ( 18.60971343765040942, 2.368090295052050820, -218.6871071987073094 ) ) ;
#19874 = CARTESIAN_POINT ( 'NONE',  ( 10.83706092800007781, 10.12544885278926543, -227.1716144446442343 ) ) ;
#19875 = CARTESIAN_POINT ( 'NONE',  ( 15.02951300086239428, -2.213105892075448278, -222.9721716646413086 ) ) ;
#19876 = TOROIDAL_SURFACE ( 'NONE', #1909, 22.63401512838748175, 3.000000000000002665 ) ;
#19877 = CIRCLE ( 'NONE', #5869, 3.000000000000002665 ) ;
#19878 = CARTESIAN_POINT ( 'NONE',  ( -28.05279008194460744, 4.018900919424986284, -224.6698354068587662 ) ) ;
#19879 = CARTESIAN_POINT ( 'NONE',  ( 10.81638188557560731, 14.98959006186633403, -234.2424515599453514 ) ) ;
#19880 = CARTESIAN_POINT ( 'NONE',  ( -24.86519201702800430, 2.611873406124941788, -9.658447518498306295 ) ) ;
#19881 = CARTESIAN_POINT ( 'NONE',  ( 14.95414693437772868, 8.262206471704862665, -230.1862972580043163 ) ) ;
#19882 = DIRECTION ( 'NONE',  ( 1.000000000000000000, 0.000000000000000000, 0.000000000000000000 ) ) ;
#19883 = CARTESIAN_POINT ( 'NONE',  ( 17.64863983146639015, -7.217312291206318342, -219.9249463058993399 ) ) ;
#19884 = CARTESIAN_POINT ( 'NONE',  ( -14.76273180397945772, -6.370707202906876532, -220.0066229284273334 ) ) ;
#19885 = CARTESIAN_POINT ( 'NONE',  ( -22.57082077310269952, -4.464701546683219391, -8.971916582499627424 ) ) ;
#19886 = DIRECTION ( 'NONE',  ( -1.000000000000000000, 0.000000000000000000, 0.000000000000000000 ) ) ;
#19887 = CARTESIAN_POINT ( 'NONE',  ( -8.523771322135640816, 24.09653697920728987, -233.1071395647740303 ) ) ;
#19888 = CARTESIAN_POINT ( 'NONE',  ( 15.43677305580571435, -6.701975615562529853, -215.9934368197604897 ) ) ;
#19889 = AXIS2_PLACEMENT_3D ( 'NONE', #1540, #2774, #4795 ) ;
#19890 = CARTESIAN_POINT ( 'NONE',  ( 20.89700225552940793, -4.547446057044195911, -232.3806459760843666 ) ) ;
#19891 = CARTESIAN_POINT ( 'NONE',  ( -18.05576253097465766, 2.935622250037499104, -232.1557308718028594 ) ) ;
#19892 = CARTESIAN_POINT ( 'NONE',  ( 13.93840998928060415, 0.7705246578886114639, -220.8158265847476116 ) ) ;
#19893 = CARTESIAN_POINT ( 'NONE',  ( 14.72046356508972309, 21.23077830076469041, -229.4562045376679578 ) ) ;
#19894 = EDGE_CURVE ( 'NONE', #1644, #19076, #1548, .T. ) ;
#19895 = ORIENTED_EDGE ( 'NONE', *, *, #1646, .F. ) ;
#19896 = CARTESIAN_POINT ( 'NONE',  ( 3.878020530997904114, -17.84699472038997214, -232.6985457136631794 ) ) ;
#19897 = CARTESIAN_POINT ( 'NONE',  ( 1.701984465643877398, 14.42982486328545555, 93.00000000000002842 ) ) ;
#19898 = CARTESIAN_POINT ( 'NONE',  ( -28.88770769694534479, 14.24820799418726480, -223.2044777450442155 ) ) ;
#19899 = CARTESIAN_POINT ( 'NONE',  ( -4.678665819194652187, 12.50541869316310262, -220.1509054161798247 ) ) ;
#19900 = CARTESIAN_POINT ( 'NONE',  ( 6.839751633953758514, 19.11639828585652623, -235.1218211620789873 ) ) ;
#19901 = CARTESIAN_POINT ( 'NONE',  ( 18.69377297094946755, -6.763382089143314957, -232.1160126380615338 ) ) ;
#19902 = CARTESIAN_POINT ( 'NONE',  ( -10.24288955603410933, 28.30762631303078791, -220.8855665231519083 ) ) ;
#19903 = CARTESIAN_POINT ( 'NONE',  ( -0.1235481402557490893, -14.50024104873819830, 92.99999999999998579 ) ) ;
#19904 = CARTESIAN_POINT ( 'NONE',  ( -6.094651895680649467, 13.59752566126439177, -221.0608041154719103 ) ) ;
#19905 = CARTESIAN_POINT ( 'NONE',  ( -15.82952867276381603, 3.677461268355039170, -227.9997968350711801 ) ) ;
#19906 =( REPRESENTATION_RELATIONSHIP ('NONE','NONE', #5277, #13052 ) REPRESENTATION_RELATIONSHIP_WITH_TRANSFORMATION ( #6575 )SHAPE_REPRESENTATION_RELATIONSHIP( ) );
#19907 = CARTESIAN_POINT ( 'NONE',  ( -10.30050448363967419, 10.07750059423401190, -220.1837019037183723 ) ) ;
#19908 = CARTESIAN_POINT ( 'NONE',  ( 25.69300549816939494, 5.947472783069708946, -230.6131061331718115 ) ) ;
#19909 = CARTESIAN_POINT ( 'NONE',  ( 6.402706778685327116, 14.41397785959879307, -226.0127495172349086 ) ) ;
#19910 = DIRECTION ( 'NONE',  ( -1.000000000000000000, 0.000000000000000000, 0.000000000000000000 ) ) ;
#19911 = CARTESIAN_POINT ( 'NONE',  ( 13.55451907249704213, 16.71566520821242818, -219.1474322952048226 ) ) ;
#19912 = CARTESIAN_POINT ( 'NONE',  ( -24.92024473536680773, -13.74570206812420103, -220.1598944320903115 ) ) ;
#19913 = CARTESIAN_POINT ( 'NONE',  ( 22.66390650824515873, 11.48342577402021725, -231.3155567808436217 ) ) ;
#19914 = CARTESIAN_POINT ( 'NONE',  ( 0.1236778125412633655, -13.14499247612405775, -221.8775184276742323 ) ) ;
#19915 = FACE_OUTER_BOUND ( 'NONE', #961, .T. ) ;
#19916 = CARTESIAN_POINT ( 'NONE',  ( -7.965409144353247761, 13.56739834143082213, -221.6246244520798712 ) ) ;
#19917 = ADVANCED_FACE ( 'NONE', ( #9561 ), #998, .F. ) ;
#19918 = CARTESIAN_POINT ( 'NONE',  ( 13.09169075717699293, -6.869491136113572871, -220.8313809912125691 ) ) ;
#19919 = CARTESIAN_POINT ( 'NONE',  ( 20.54489901492447501, 10.52141067440427591, -216.2005526543161693 ) ) ;
#19920 = CARTESIAN_POINT ( 'NONE',  ( -16.12870690754239078, 23.19263481078822053, -221.6099859194323471 ) ) ;
#19921 = CARTESIAN_POINT ( 'NONE',  ( -15.42311360645077301, 11.97619046995196079, -234.9244673706848801 ) ) ;
#19922 = CARTESIAN_POINT ( 'NONE',  ( -18.83136555461844708, -9.493528738360442532, -219.1308048892593945 ) ) ;
#19923 = CARTESIAN_POINT ( 'NONE',  ( -15.94549496081242346, -0.04271059606100771622, -224.7066567765017169 ) ) ;
#19924 = STYLED_ITEM ( 'NONE', ( #12435 ), #14254 ) ;
#19925 =( GEOMETRIC_REPRESENTATION_CONTEXT ( 3 ) GLOBAL_UNCERTAINTY_ASSIGNED_CONTEXT ( ( #22011 ) ) GLOBAL_UNIT_ASSIGNED_CONTEXT ( ( #2998, #21681, #8013 ) ) REPRESENTATION_CONTEXT ( 'NONE', 'WORKASPACE' ) );
#19926 = DIRECTION ( 'NONE',  ( -1.000000000000000000, 0.000000000000000000, 0.000000000000000000 ) ) ;
#19927 = CARTESIAN_POINT ( 'NONE',  ( -23.12176686270140991, -7.251528982847554872, -234.5139663548038413 ) ) ;
#19928 = CARTESIAN_POINT ( 'NONE',  ( 2.471164685565028662, 14.01327037412690935, -223.4905256513065410 ) ) ;
#19929 = CARTESIAN_POINT ( 'NONE',  ( 25.62718606866737403, 13.33219119508369310, -230.9315691959737933 ) ) ;
#19930 = CARTESIAN_POINT ( 'NONE',  ( -18.09605518090995702, 22.22778748761825085, -222.5443354630425290 ) ) ;
#19931 = CARTESIAN_POINT ( 'NONE',  ( 11.20580770355584299, 27.81589616365139150, -231.3138133330081132 ) ) ;
#19932 = VERTEX_POINT ( 'NONE', #4475 ) ;
#19933 = CARTESIAN_POINT ( 'NONE',  ( 8.192339082998598698, -27.06056373437490947, -224.5174968915583236 ) ) ;
#19934 = ORIENTED_EDGE ( 'NONE', *, *, #21643, .T. ) ;
#19935 = CARTESIAN_POINT ( 'NONE',  ( 1.632321987819951969, -14.78074153629778387, -224.5834756332612301 ) ) ;
#19936 = CARTESIAN_POINT ( 'NONE',  ( -31.76239872120898511, 5.177298019713663990, -226.5714959923072342 ) ) ;
#19937 = CARTESIAN_POINT ( 'NONE',  ( 15.54083024098960486, -10.44392130763852222, -217.6620978190037476 ) ) ;
#19938 = CARTESIAN_POINT ( 'NONE',  ( 26.86542643433637423, 1.561297562127881511, -231.3515426572852505 ) ) ;
#19939 = AXIS2_PLACEMENT_3D ( 'NONE', #12495, #19342, #3924 ) ;
#19940 = CARTESIAN_POINT ( 'NONE',  ( -21.63546480557098306, -21.44004028177477750, -223.8762611443524122 ) ) ;
#19941 = AXIS2_PLACEMENT_3D ( 'NONE', #14682, #4531, #21516 ) ;
#19942 = CARTESIAN_POINT ( 'NONE',  ( 3.174664235197445006, 17.30896320251298448, -221.0803896709622620 ) ) ;
#19943 = CARTESIAN_POINT ( 'NONE',  ( -14.98215928292561294, 22.79623052288931362, -230.3289734367122890 ) ) ;
#19944 = CARTESIAN_POINT ( 'NONE',  ( 11.82943521288609823, 27.58963564415041247, -226.1180395413371400 ) ) ;
#19945 = CARTESIAN_POINT ( 'NONE',  ( 7.487569386194327770, 15.49107591903592862, -229.0624668269501001 ) ) ;
#19946 = CARTESIAN_POINT ( 'NONE',  ( 19.49551695935633688, -21.73806820219217428, -217.5227155576580742 ) ) ;
#19947 = CARTESIAN_POINT ( 'NONE',  ( 8.379126514044342500, 15.76264856365358646, -232.1787896114811360 ) ) ;
#19948 = CARTESIAN_POINT ( 'NONE',  ( -12.70465517376339193, 12.03139199664008530, -229.6235454691090752 ) ) ;
#19949 = CARTESIAN_POINT ( 'NONE',  ( -15.72195651633673208, 2.938252489821347346, -222.2698596109374023 ) ) ;
#19950 = CARTESIAN_POINT ( 'NONE',  ( -1.981531036097845533, -15.05108582582333909, -227.0172948689592829 ) ) ;
#19951 = CARTESIAN_POINT ( 'NONE',  ( 0.000000000000000000, 0.000000000000000000, -105.0000000000000142 ) ) ;
#19952 = DIRECTION ( 'NONE',  ( -1.000000000000000000, 0.000000000000000000, 0.000000000000000000 ) ) ;
#19953 = EDGE_CURVE ( 'NONE', #6126, #2334, #21242, .T. ) ;
#19954 = CARTESIAN_POINT ( 'NONE',  ( 12.58590500897257947, 11.38573988265384607, -230.4867078522624695 ) ) ;
#19955 = CARTESIAN_POINT ( 'NONE',  ( 10.38773686668317531, -11.52324865342443516, -226.2052026729718932 ) ) ;
#19956 = DIRECTION ( 'NONE',  ( 0.000000000000000000, 1.000000000000000000, -0.000000000000000000 ) ) ;
#19957 = VECTOR ( 'NONE', #21493, 1000.000000000000000 ) ;
#19958 = CARTESIAN_POINT ( 'NONE',  ( -8.258403559667634397, -29.80786866836635696, -223.3983869762195127 ) ) ;
#19959 = SHAPE_DEFINITION_REPRESENTATION ( #1694, #13052 ) ;
#19960 = CARTESIAN_POINT ( 'NONE',  ( -2.958555384449997661, 13.07587799061801093, -222.7767538261418565 ) ) ;
#19961 = CARTESIAN_POINT ( 'NONE',  ( 3.889974896201825239, 13.98719620150063214, -218.1465764473210527 ) ) ;
#19962 = ORIENTED_EDGE ( 'NONE', *, *, #15957, .T. ) ;
#19963 = CARTESIAN_POINT ( 'NONE',  ( -3.843007962268670585, 27.94983497691806917, -231.4302614368887703 ) ) ;
#19964 = CARTESIAN_POINT ( 'NONE',  ( -23.30703516638871875, -0.6243632158918477337, -216.1214812734271220 ) ) ;
#19965 = CARTESIAN_POINT ( 'NONE',  ( -24.60379713026238235, -4.442902817157290407, 8.964804537911287952 ) ) ;
#19966 = DIRECTION ( 'NONE',  ( -1.000000000000000000, 0.000000000000000000, 2.891205793294678696E-17 ) ) ;
#19967 = CARTESIAN_POINT ( 'NONE',  ( -11.49049084071896409, 11.06834963248926940, -218.3354249205727058 ) ) ;
#19968 = CARTESIAN_POINT ( 'NONE',  ( -21.30077981517617047, -23.37245693150986270, -228.9371924788557351 ) ) ;
#19969 = CARTESIAN_POINT ( 'NONE',  ( 14.68556740487494849, -6.365102927765655672, -229.6664356779805587 ) ) ;
#19970 = CARTESIAN_POINT ( 'NONE',  ( -8.966714183099560032, 19.05224306381768073, -234.0879867025980445 ) ) ;
#19971 = CARTESIAN_POINT ( 'NONE',  ( 19.10353041285295816, 2.510539514498965730, -232.1135168369976896 ) ) ;
#19972 = CARTESIAN_POINT ( 'NONE',  ( 1.430961520682887400, 16.89318350835024063, -220.3256763723340157 ) ) ;
#19973 = LINE ( 'NONE', #18527, #14836 ) ;
#19974 = CARTESIAN_POINT ( 'NONE',  ( 18.14488609917747652, 6.993670804558928644, -231.4804853770579882 ) ) ;
#19975 = CARTESIAN_POINT ( 'NONE',  ( -8.698852260299409167, -27.05211559305675451, -224.0453856107860986 ) ) ;
#19976 = VECTOR ( 'NONE', #9365, 1000.000000000000000 ) ;
#19977 = VERTEX_POINT ( 'NONE', #1332 ) ;
#19978 = CARTESIAN_POINT ( 'NONE',  ( -10.16319438574952372, 11.71174522937666040, -227.8434026503654479 ) ) ;
#19979 = CARTESIAN_POINT ( 'NONE',  ( 21.26803326031697949, 19.54255073453192892, -230.5813148908474659 ) ) ;
#19980 = CARTESIAN_POINT ( 'NONE',  ( -5.786930954831501772, 15.78543306641166311, -231.0475152612371517 ) ) ;
#19981 = CARTESIAN_POINT ( 'NONE',  ( -25.99367553232993799, -4.794975032520305547, -231.0351783075731191 ) ) ;
#19982 = FACE_OUTER_BOUND ( 'NONE', #3274, .T. ) ;
#19983 = ORIENTED_EDGE ( 'NONE', *, *, #6596, .T. ) ;
#19984 = CARTESIAN_POINT ( 'NONE',  ( -9.171998067665157350, 9.395241133357435714, -226.3428046914542051 ) ) ;
#19985 = CARTESIAN_POINT ( 'NONE',  ( -5.577337716965932835, -27.36628652700976971, -219.4670492756933413 ) ) ;
#19986 = CARTESIAN_POINT ( 'NONE',  ( 15.50884165284638705, 1.028647572718199843, -227.8181348745474679 ) ) ;
#19987 = CARTESIAN_POINT ( 'NONE',  ( 11.82943521288609823, 27.58963564415041247, -226.1180395413371400 ) ) ;
#19988 = FACE_OUTER_BOUND ( 'NONE', #13582, .T. ) ;
#19989 = UNCERTAINTY_MEASURE_WITH_UNIT (LENGTH_MEASURE( 1.000000000000000082E-05 ), #1634, 'distance_accuracy_value', 'NONE');
#19990 = CARTESIAN_POINT ( 'NONE',  ( -15.46752262371512820, 15.15798787883389487, -233.5981584775992701 ) ) ;
#19991 = CARTESIAN_POINT ( 'NONE',  ( 21.18605525173251891, 3.426801613781890854, -232.1183243183448894 ) ) ;
#19992 = CARTESIAN_POINT ( 'NONE',  ( 15.34286276367735979, 1.557318373440422565, -222.4358706187587416 ) ) ;
#19993 = EDGE_CURVE ( 'NONE', #6969, #22262, #11599, .T. ) ;
#19994 = CARTESIAN_POINT ( 'NONE',  ( 16.07305932912010960, 0.9253679043337685872, -229.0409936706996064 ) ) ;
#19995 = CARTESIAN_POINT ( 'NONE',  ( -19.63401512838757057, 1.925929944387226885E-29, -77.51594804401857175 ) ) ;
#19996 = CARTESIAN_POINT ( 'NONE',  ( 26.20608998270887469, -2.199599969171641689, -229.6935040011478009 ) ) ;
#19997 = CARTESIAN_POINT ( 'NONE',  ( -21.80830016239255897, -4.781675611938959847, -217.4666014280278148 ) ) ;
#19998 = EDGE_CURVE ( 'NONE', #11225, #15441, #5132, .T. ) ;
#19999 = CARTESIAN_POINT ( 'NONE',  ( 1.526556658859590243E-13, -21.00000000000000000, -75.00000000000000000 ) ) ;
#20000 = FACE_OUTER_BOUND ( 'NONE', #5007, .T. ) ;
#20001 = CARTESIAN_POINT ( 'NONE',  ( -1.565160934061885500, 18.19073094521525391, -232.0278805765578909 ) ) ;
#20002 = CARTESIAN_POINT ( 'NONE',  ( 20.64894435305043174, -4.471500992710556233, -235.2405168901568686 ) ) ;
#20003 = CARTESIAN_POINT ( 'NONE',  ( 23.48720700658024896, -2.145453947144424500, -217.8824464111000054 ) ) ;
#20004 = CARTESIAN_POINT ( 'NONE',  ( -24.39036648059286350, 13.21953970265592027, -220.1632778389106591 ) ) ;
#20005 = CARTESIAN_POINT ( 'NONE',  ( -19.11923763334766946, 1.257783214997954202, -219.7591028439344711 ) ) ;
#20006 = CARTESIAN_POINT ( 'NONE',  ( 9.322595869360968734, 23.38184458253662967, -230.2763482547081821 ) ) ;
#20007 = CARTESIAN_POINT ( 'NONE',  ( -0.3443283949127196042, -14.50397496964243516, -224.4114361181996458 ) ) ;
#20008 = CARTESIAN_POINT ( 'NONE',  ( 0.8583760989383623086, 14.48452571672253519, 93.00000000000000000 ) ) ;
#20009 = CARTESIAN_POINT ( 'NONE',  ( -13.06407726305387307, 3.888674610242962348, -219.0371145420960204 ) ) ;
#20010 = CARTESIAN_POINT ( 'NONE',  ( 19.29971334243027314, 24.42889259816135095, -228.2141526116784291 ) ) ;
#20011 = CARTESIAN_POINT ( 'NONE',  ( 0.6332696906856497554, 18.74964962670039625, -234.8596399859513042 ) ) ;
#20012 = CARTESIAN_POINT ( 'NONE',  ( 18.71980393303116230, -12.14054210360577457, -231.5113610204687120 ) ) ;
#20013 = CARTESIAN_POINT ( 'NONE',  ( -2.958555384449997661, 13.07587799061801093, -222.7767538261418565 ) ) ;
#20014 = CARTESIAN_POINT ( 'NONE',  ( -14.70651859537745487, 4.211702956367679107, -230.0357207626005334 ) ) ;
#20015 = ADVANCED_FACE ( 'NONE', ( #11568 ), #10416, .T. ) ;
#20016 = CARTESIAN_POINT ( 'NONE',  ( 19.07698357483942786, 25.86742807064150895, -222.6991278896559834 ) ) ;
#20017 = CARTESIAN_POINT ( 'NONE',  ( -24.49083850720273148, 4.222094140707651100, -219.1543001448025905 ) ) ;
#20018 = CARTESIAN_POINT ( 'NONE',  ( -12.78558550453068854, 7.693178343823584342, -230.0800953344970878 ) ) ;
#20019 = CARTESIAN_POINT ( 'NONE',  ( 27.40550551777678123, 5.967061366481472895, -228.7463788799179554 ) ) ;
#20020 = CARTESIAN_POINT ( 'NONE',  ( 3.191455400233187412, 17.67480163422566619, -220.7055581859663107 ) ) ;
#20021 = DIRECTION ( 'NONE',  ( 4.845403715540905824E-30, -6.938893903907257960E-16, 1.000000000000000000 ) ) ;
#20022 = DIRECTION ( 'NONE',  ( 0.000000000000000000, 0.000000000000000000, -1.000000000000000000 ) ) ;
#20023 = CARTESIAN_POINT ( 'NONE',  ( 16.29563576379945999, 21.41235115595959826, -221.8114656550040991 ) ) ;
#20024 = CARTESIAN_POINT ( 'NONE',  ( -9.078153229956912540, -10.71731945587431056, -228.5228069477245469 ) ) ;
#20025 = CARTESIAN_POINT ( 'NONE',  ( 22.86997486125673618, 17.56009411325475966, -222.3578648042903296 ) ) ;
#20026 = CARTESIAN_POINT ( 'NONE',  ( -0.1378336831626507664, -14.33879523207274964, -230.9095596798049144 ) ) ;
#20027 = DIRECTION ( 'NONE',  ( 0.000000000000000000, 0.000000000000000000, 1.000000000000000000 ) ) ;
#20028 = CARTESIAN_POINT ( 'NONE',  ( -15.51982305277792307, 19.76957551617798359, -231.4018974401358832 ) ) ;
#20029 = SURFACE_STYLE_FILL_AREA ( #18141 ) ;
#20030 = CARTESIAN_POINT ( 'NONE',  ( 12.85536293311005451, -7.423602990911125410, -229.4216632760384300 ) ) ;
#20031 = CARTESIAN_POINT ( 'NONE',  ( 20.88350594575732799, 13.65521425050155813, -232.8060468608549911 ) ) ;
#20032 = CARTESIAN_POINT ( 'NONE',  ( -4.879985665934096772, 15.33285679834440174, -220.9402849574511833 ) ) ;
#20033 = CARTESIAN_POINT ( 'NONE',  ( -12.13319425917249283, 4.024026700415168634, -229.5243363405849095 ) ) ;
#20034 = CARTESIAN_POINT ( 'NONE',  ( -26.46950597041758968, -8.633348373924491170, -225.4226425040951085 ) ) ;
#20035 = CARTESIAN_POINT ( 'NONE',  ( -25.48569860171343748, 4.299098795181173216, -219.7804659532078801 ) ) ;
#20036 = EDGE_CURVE ( 'NONE', #12003, #12810, #8384, .T. ) ;
#20037 = CARTESIAN_POINT ( 'NONE',  ( 0.000000000000000000, 21.80000000000000071, 78.50000000000000000 ) ) ;
#20038 = CARTESIAN_POINT ( 'NONE',  ( -27.95235446785429545, -6.124178816625678756, -218.3296603670965226 ) ) ;
#20039 = CARTESIAN_POINT ( 'NONE',  ( 10.88376588832297287, 7.577514201227793400, -222.7215714477710833 ) ) ;
#20040 = CARTESIAN_POINT ( 'NONE',  ( 18.81274554574540403, 10.85963742466947224, -234.0446454529665345 ) ) ;
#20041 = CARTESIAN_POINT ( 'NONE',  ( -2.121548062149551495, 13.26065194155116345, -221.8830439064491884 ) ) ;
#20042 = CARTESIAN_POINT ( 'NONE',  ( 7.739849882373770917, 11.59357455229016409, -219.5521933286238720 ) ) ;
#20043 = CARTESIAN_POINT ( 'NONE',  ( 0.5565384680698680642, -16.73444667301361122, -219.8404036742738015 ) ) ;
#20044 = ORIENTED_EDGE ( 'NONE', *, *, #9377, .F. ) ;
#20045 = CARTESIAN_POINT ( 'NONE',  ( 0.7797512750231831991, -26.58197935702783354, -230.4407411870234625 ) ) ;
#20046 = CIRCLE ( 'NONE', #5317, 3.000000000000030198 ) ;
#20047 = CARTESIAN_POINT ( 'NONE',  ( -10.54177647804913320, 7.401649028325941515, -220.3980514230326264 ) ) ;
#20048 = CARTESIAN_POINT ( 'NONE',  ( 20.25084204406298127, -10.11176871144018818, -232.7817218064674591 ) ) ;
#20049 = CARTESIAN_POINT ( 'NONE',  ( -27.09167109716269550, -0.2825935922571593539, -219.8389404328913486 ) ) ;
#20050 = CARTESIAN_POINT ( 'NONE',  ( -6.012234575298915473, -13.00555924700598709, -229.4955436083688483 ) ) ;
#20051 = CARTESIAN_POINT ( 'NONE',  ( 17.98704291748025952, 16.14142602298251461, -217.3684083235702644 ) ) ;
#20052 = DIRECTION ( 'NONE',  ( -0.000000000000000000, -0.000000000000000000, 1.000000000000000000 ) ) ;
#20053 = CARTESIAN_POINT ( 'NONE',  ( -22.57344584932824105, 14.14390280519600473, -217.2212543695777924 ) ) ;
#20054 = CARTESIAN_POINT ( 'NONE',  ( 8.645835506124264214, 12.38899589144949687, -223.4673650485651990 ) ) ;
#20055 = CARTESIAN_POINT ( 'NONE',  ( 10.02513374692848913, 18.81568788741115128, -217.1505009242214612 ) ) ;
#20056 = CARTESIAN_POINT ( 'NONE',  ( 14.91731358302415877, 13.33846450914490056, -217.2468882285060658 ) ) ;
#20057 = CARTESIAN_POINT ( 'NONE',  ( 14.18953136290653205, -9.569333121228954298, -216.2179364387266389 ) ) ;
#20058 = CARTESIAN_POINT ( 'NONE',  ( 13.10956039622986324, 4.581323766968698585, -221.0328522389722252 ) ) ;
#20059 = CARTESIAN_POINT ( 'NONE',  ( -11.69222874857179484, 25.57550432052970280, -219.9467848335519591 ) ) ;
#20060 = CARTESIAN_POINT ( 'NONE',  ( -13.02663300398358892, -17.15584419188240162, -232.5492131852532793 ) ) ;
#20061 = CARTESIAN_POINT ( 'NONE',  ( -23.00000000000000000, 0.000000000000000000, 75.00000000000000000 ) ) ;
#20062 = DIRECTION ( 'NONE',  ( 1.000000000000000000, 0.000000000000000000, 0.000000000000000000 ) ) ;
#20063 = CARTESIAN_POINT ( 'NONE',  ( 24.42567939027770407, 10.22651298688739097, -219.4562066833365748 ) ) ;
#20064 = CARTESIAN_POINT ( 'NONE',  ( 22.17529396115045870, -12.37645153867399195, -229.8268438261158906 ) ) ;
#20065 = CARTESIAN_POINT ( 'NONE',  ( -13.51406939156936104, 10.04301168678160749, -230.1761202643687056 ) ) ;
#20066 = CIRCLE ( 'NONE', #8941, 22.92944763917984474 ) ;
#20067 = CARTESIAN_POINT ( 'NONE',  ( -5.902479482706956659, -14.78727544128710214, -218.5565286504736946 ) ) ;
#20068 = CARTESIAN_POINT ( 'NONE',  ( 29.55842656951424985, 4.785221541509360854, -220.5134865854112718 ) ) ;
#20069 = CARTESIAN_POINT ( 'NONE',  ( 4.569118550756183339, 31.72363458735121000, -222.3920438419263519 ) ) ;
#20070 = ORIENTED_EDGE ( 'NONE', *, *, #12449, .T. ) ;
#20071 = CARTESIAN_POINT ( 'NONE',  ( 3.449504654906655254, 27.59247159270940841, -231.3461799890608859 ) ) ;
#20072 = CARTESIAN_POINT ( 'NONE',  ( -15.34124043857492303, -4.213426711746545372, -218.8308339851419078 ) ) ;
#20073 = CARTESIAN_POINT ( 'NONE',  ( -23.18452556481357618, -9.353925523610076453, -3.551024142333974787 ) ) ;
#20074 = CARTESIAN_POINT ( 'NONE',  ( -6.938893903907228378E-15, 0.000000000000000000, -224.9999999999999716 ) ) ;
#20075 = CARTESIAN_POINT ( 'NONE',  ( 4.301648988406530094, 13.23079486486395240, -223.2766268961034655 ) ) ;
#20076 = CARTESIAN_POINT ( 'NONE',  ( -6.608244874605412100, -9.640126028631323507, -223.8427097396816805 ) ) ;
#20077 = CARTESIAN_POINT ( 'NONE',  ( 6.427665535191954937, -16.40046818492683656, -232.5919299485929912 ) ) ;
#20078 = CARTESIAN_POINT ( 'NONE',  ( 13.49882595795384255, -9.201056071450322449, -219.2439763087855908 ) ) ;
#20079 = CARTESIAN_POINT ( 'NONE',  ( -14.64425879132321384, 10.88727730234500868, -217.2315376225554644 ) ) ;
#20080 = CARTESIAN_POINT ( 'NONE',  ( 10.12648780932046755, 24.76571117977573522, -228.8499436907259792 ) ) ;
#20081 = CARTESIAN_POINT ( 'NONE',  ( 0.000000000000000000, 0.000000000000000000, -75.00000000000000000 ) ) ;
#20082 = CARTESIAN_POINT ( 'NONE',  ( -10.10782416658048710, 9.083762506436128703, -227.1045422723873344 ) ) ;
#20083 = CARTESIAN_POINT ( 'NONE',  ( -13.53417258903678722, -8.044363197357762729, -224.1542709308240546 ) ) ;
#20084 = CARTESIAN_POINT ( 'NONE',  ( -21.66803296057637951, 19.04503900041684616, -222.6603677762044526 ) ) ;
#20085 = CARTESIAN_POINT ( 'NONE',  ( 17.23498165643884761, 6.576565757823654934, -216.5785374982484655 ) ) ;
#20086 = CARTESIAN_POINT ( 'NONE',  ( 2.000982021813747291, 12.72833461843010205, -228.3416607300594308 ) ) ;
#20087 = CARTESIAN_POINT ( 'NONE',  ( -17.40151406155100844, -6.170051014037699844, -218.8120118016391871 ) ) ;
#20088 = DIRECTION ( 'NONE',  ( 1.000000000000000000, 0.000000000000000000, 0.000000000000000000 ) ) ;
#20089 = VERTEX_POINT ( 'NONE', #11685 ) ;
#20090 = CARTESIAN_POINT ( 'NONE',  ( -14.07917727715460821, 7.534853284453274291, -218.6337090155677458 ) ) ;
#20091 = CARTESIAN_POINT ( 'NONE',  ( -13.20345004609422723, -27.40577205094947644, -221.7016714442654290 ) ) ;
#20092 = CARTESIAN_POINT ( 'NONE',  ( 15.88514075556662242, 1.727533893982488244, -221.2479562541981011 ) ) ;
#20093 = CARTESIAN_POINT ( 'NONE',  ( 15.85665641241444668, 18.24713744004561988, -217.7195292979064902 ) ) ;
#20094 = LINE ( 'NONE', #14952, #7342 ) ;
#20095 = CARTESIAN_POINT ( 'NONE',  ( 22.03647168421188240, 0.3315607655626218175, -232.0572713672587213 ) ) ;
#20096 = CARTESIAN_POINT ( 'NONE',  ( -11.19223248830523332, 8.463078350427430507, -222.6400917074981578 ) ) ;
#20097 = CARTESIAN_POINT ( 'NONE',  ( 14.70646826691583975, 6.155951851203820269, -230.2899142379868920 ) ) ;
#20098 = CARTESIAN_POINT ( 'NONE',  ( 15.23010956230245228, 0.3844360911890600807, -222.0229298927499713 ) ) ;
#20099 = CARTESIAN_POINT ( 'NONE',  ( 19.38184807124232378, -2.462809743167423626, -223.2754647498610154 ) ) ;
#20100 = CARTESIAN_POINT ( 'NONE',  ( -21.89065952084848021, -0.9940043559354364566, -216.9999999999999716 ) ) ;
#20101 = CARTESIAN_POINT ( 'NONE',  ( 18.18465861704851960, -5.084991117879029687, -230.0453011691623999 ) ) ;
#20103 = EDGE_CURVE ( 'NONE', #8392, #10586, #7044, .T. ) ;
#20102 = CARTESIAN_POINT ( 'NONE',  ( -26.98579662683621194, -8.531126968542736222, -229.5232528995939845 ) ) ;
#20104 = CARTESIAN_POINT ( 'NONE',  ( 0.000000000000000000, 0.000000000000000000, -120.0000000000000142 ) ) ;
#20105 = CARTESIAN_POINT ( 'NONE',  ( 0.000000000000000000, 21.80000000000006111, 78.50000000000000000 ) ) ;
#20106 = CARTESIAN_POINT ( 'NONE',  ( 9.322595869360968734, 23.38184458253662967, -230.2763482547081821 ) ) ;
#20107 = CARTESIAN_POINT ( 'NONE',  ( 12.92460608403495037, -28.21656386930617089, -223.0937501850342812 ) ) ;
#20108 = CARTESIAN_POINT ( 'NONE',  ( 12.02378739738799140, -16.98783239109716092, -233.4545636224233931 ) ) ;
#20109 = CARTESIAN_POINT ( 'NONE',  ( -22.13857085231108712, 6.545953331035805789, -217.2801712530867633 ) ) ;
#20110 = CARTESIAN_POINT ( 'NONE',  ( 16.21758812354607215, 4.665393561625732488, -232.5634757513959983 ) ) ;
#20111 = CARTESIAN_POINT ( 'NONE',  ( 15.04029996350473830, 7.457450192165341107, -220.5007084872782173 ) ) ;
#20112 = CARTESIAN_POINT ( 'NONE',  ( 2.920206608988989760, -13.21961856575012639, -224.5557534934820865 ) ) ;
#20113 = CARTESIAN_POINT ( 'NONE',  ( -13.09048442463468120, -0.002406630494250819839, -229.7150300986316438 ) ) ;
#20114 = CARTESIAN_POINT ( 'NONE',  ( 3.889974896201825239, 13.98719620150063214, -218.1465764473210527 ) ) ;
#20115 = CARTESIAN_POINT ( 'NONE',  ( 3.889974896201825239, 13.98719620150063214, -218.1465764473210527 ) ) ;
#20116 = CARTESIAN_POINT ( 'NONE',  ( 22.50501984129641286, -15.15275112778533284, -228.8333022290248664 ) ) ;
#20117 = EDGE_CURVE ( 'NONE', #20783, #20366, #18080, .T. ) ;
#20118 = CARTESIAN_POINT ( 'NONE',  ( -9.517741096562200909, 20.63709896626785678, -234.1036702156204967 ) ) ;
#20119 = CARTESIAN_POINT ( 'NONE',  ( -17.96792326766206926, -0.6237852504629022299, -217.9759415197746932 ) ) ;
#20120 = CARTESIAN_POINT ( 'NONE',  ( 8.126072675580726212, 14.68573014611672534, -233.8823376361746966 ) ) ;
#20121 = CARTESIAN_POINT ( 'NONE',  ( -15.10945752141584464, 6.470132813599071220, -220.1568141593501764 ) ) ;
#20122 = CARTESIAN_POINT ( 'NONE',  ( -3.003186468682855104, 15.63968344752823469, -231.5301608670590667 ) ) ;
#20123 = CARTESIAN_POINT ( 'NONE',  ( 6.539635590297932843, 8.674798497629369720, 92.00000000000001421 ) ) ;
#20124 = CARTESIAN_POINT ( 'NONE',  ( 7.042184411928968935, 23.28260216771182556, -230.5707103145148267 ) ) ;
#20125 = FACE_OUTER_BOUND ( 'NONE', #7107, .T. ) ;
#20126 = CARTESIAN_POINT ( 'NONE',  ( -23.00000000000000000, 0.000000000000000000, -55.00000000000000000 ) ) ;
#20127 = CARTESIAN_POINT ( 'NONE',  ( -24.25245498015852874, 0.2109992039763788352, -218.1398602137601301 ) ) ;
#20128 = CARTESIAN_POINT ( 'NONE',  ( 24.57222455393806015, 12.08236629421828212, -229.7319216558644541 ) ) ;
#20129 = CARTESIAN_POINT ( 'NONE',  ( -11.33724117040414647, -11.57131516804904159, -228.9094961685112537 ) ) ;
#20130 = CARTESIAN_POINT ( 'NONE',  ( -9.810154340578240095, 25.84808829058669488, -220.5759521898573610 ) ) ;
#20131 = FILL_AREA_STYLE_COLOUR ( '', #14239 ) ;
#20132 = CARTESIAN_POINT ( 'NONE',  ( 12.74640035234706659, -6.767230903810586895, -221.4971111014800726 ) ) ;
#20133 = CARTESIAN_POINT ( 'NONE',  ( 14.29768887814754663, 10.87030385293788548, -231.8067013864770161 ) ) ;
#20134 = CARTESIAN_POINT ( 'NONE',  ( -4.130417896617784912, 16.21758012034559826, -229.8171973319304584 ) ) ;
#20135 = CARTESIAN_POINT ( 'NONE',  ( -14.00980274651940682, 20.05588230486321066, -234.2453272803952586 ) ) ;
#20136 = VERTEX_POINT ( 'NONE', #8845 ) ;
#20137 = CARTESIAN_POINT ( 'NONE',  ( -16.09622215267033596, -6.362375831002168525, -228.5323951500822943 ) ) ;
#20138 = CARTESIAN_POINT ( 'NONE',  ( 14.81251837262747983, -1.020578734748967209, -221.0290343291311785 ) ) ;
#20139 = DIRECTION ( 'NONE',  ( 0.000000000000000000, 0.000000000000000000, -1.000000000000000000 ) ) ;
#20140 = CARTESIAN_POINT ( 'NONE',  ( -26.73251495235368225, -0.6309583860051256599, -232.5016102969711085 ) ) ;
#20141 = CARTESIAN_POINT ( 'NONE',  ( 9.211411085256067111, 16.86455563410128633, -232.8411836211112700 ) ) ;
#20142 = CARTESIAN_POINT ( 'NONE',  ( -15.47996233766743934, 8.203483081506188768, -221.0931279926996353 ) ) ;
#20143 = CARTESIAN_POINT ( 'NONE',  ( -3.712761995161701911, 23.50704853188985766, -216.1220552374512067 ) ) ;
#20144 = CARTESIAN_POINT ( 'NONE',  ( 14.70646826691583975, 6.155951851203820269, -230.2899142379868920 ) ) ;
#20145 = ORIENTED_EDGE ( 'NONE', *, *, #7567, .T. ) ;
#20146 = CARTESIAN_POINT ( 'NONE',  ( -19.56933409648781108, -21.97186532644649759, -218.6835957583845982 ) ) ;
#20147 = VERTEX_POINT ( 'NONE', #13261 ) ;
#20148 = CARTESIAN_POINT ( 'NONE',  ( -8.326748185965973548, -13.59788789161040512, -220.4531618457016862 ) ) ;
#20149 = CARTESIAN_POINT ( 'NONE',  ( -26.98548179121306845, 3.096138561569834913, -233.8324893795610251 ) ) ;
#20150 = CARTESIAN_POINT ( 'NONE',  ( 6.053458391837899910, -12.85229775019162268, -220.9645494416007523 ) ) ;
#20151 = CARTESIAN_POINT ( 'NONE',  ( -15.89118508636071958, -1.798691612803976492, -229.3605869667087234 ) ) ;
#20152 = CARTESIAN_POINT ( 'NONE',  ( -26.98579662683621194, -8.531126968542736222, -229.5232528995939845 ) ) ;
#20153 = CARTESIAN_POINT ( 'NONE',  ( 11.35656094503625901, 14.01405796444069018, -230.6944611846958537 ) ) ;
#20154 = DIRECTION ( 'NONE',  ( -0.000000000000000000, -0.000000000000000000, -1.000000000000000000 ) ) ;
#20155 = CARTESIAN_POINT ( 'NONE',  ( -8.308618357598591686, 12.44656112581930785, -228.0014162119141474 ) ) ;
#20156 = CARTESIAN_POINT ( 'NONE',  ( 11.44717363687632528, 10.34477785005100969, -220.4550508611108341 ) ) ;
#20157 = CARTESIAN_POINT ( 'NONE',  ( -2.208416658185406334, 29.10348627872611615, -219.8480645685746424 ) ) ;
#20158 = CARTESIAN_POINT ( 'NONE',  ( 6.729623925010410623, 16.84721552001897038, -219.9221131804260381 ) ) ;
#20159 = CARTESIAN_POINT ( 'NONE',  ( 9.622280932921700725, -12.40415793303572300, -216.8820201732712860 ) ) ;
#20160 = CARTESIAN_POINT ( 'NONE',  ( 0.1866476013601106043, 25.93503619265524307, -233.5574764272258790 ) ) ;
#20161 = ADVANCED_FACE ( 'NONE', ( #3642 ), #4809, .T. ) ;
#20162 = CARTESIAN_POINT ( 'NONE',  ( -10.46545893407769157, -9.768586176915025732, -226.8636372813723199 ) ) ;
#20163 = CARTESIAN_POINT ( 'NONE',  ( -13.93333636822611155, 3.327141996558931947, -221.4468162587888287 ) ) ;
#20164 = DIRECTION ( 'NONE',  ( -0.9940043559354330149, -0.1093404791528966163, -6.737719923507020479E-14 ) ) ;
#20165 = AXIS2_PLACEMENT_3D ( 'NONE', #9727, #5394, #18391 ) ;
#20166 = CARTESIAN_POINT ( 'NONE',  ( 14.19800769603076240, 4.587407146151301518, -224.2928935459285071 ) ) ;
#20167 = CARTESIAN_POINT ( 'NONE',  ( 15.80653577316150837, -24.09293983082412893, -226.7583346419201575 ) ) ;
#20168 = CARTESIAN_POINT ( 'NONE',  ( -12.87285471141929172, 9.485162256560764504, -229.1865421006261840 ) ) ;
#20169 = CARTESIAN_POINT ( 'NONE',  ( 1.656472371294090085, 27.29382523973669095, -230.4991099578876117 ) ) ;
#20170 = CARTESIAN_POINT ( 'NONE',  ( -13.52935284690462758, -5.503084506376929141, -222.3607690796775671 ) ) ;
#20171 = CARTESIAN_POINT ( 'NONE',  ( 12.88374853655145458, 4.106359831454843068, -228.1016120772327440 ) ) ;
#20172 = AXIS2_PLACEMENT_3D ( 'NONE', #19358, #14091, #20931 ) ;
#20173 = CARTESIAN_POINT ( 'NONE',  ( 12.90536070039565963, 17.66816134723717724, -234.8562535614228750 ) ) ;
#20174 = VERTEX_POINT ( 'NONE', #15711 ) ;
#20175 = CARTESIAN_POINT ( 'NONE',  ( -3.003186468682855104, 15.63968344752823469, -231.5301608670590667 ) ) ;
#20176 = CARTESIAN_POINT ( 'NONE',  ( 20.08508968036338871, -9.819972662663129626, -218.2881406113160381 ) ) ;
#20177 = CARTESIAN_POINT ( 'NONE',  ( 23.33467929415965614, -0.4823873731835089940, -233.9427286327415629 ) ) ;
#20178 = CARTESIAN_POINT ( 'NONE',  ( 0.000000000000000000, 0.000000000000000000, 78.50000000000000000 ) ) ;
#20179 = CARTESIAN_POINT ( 'NONE',  ( -0.9414827276148034496, 23.96885519606619752, -216.4491898092606164 ) ) ;
#20180 = CARTESIAN_POINT ( 'NONE',  ( -15.15491452760745439, -27.84330619910961957, -221.4571841043341180 ) ) ;
#20181 = CARTESIAN_POINT ( 'NONE',  ( 12.73130673999417795, -23.76414828096303467, -217.7386337832039942 ) ) ;
#20182 = CARTESIAN_POINT ( 'NONE',  ( 19.06435866915521515, -20.24829071055443563, -218.8318535520223804 ) ) ;
#20183 = CARTESIAN_POINT ( 'NONE',  ( -11.83206531956964902, 10.60028422373495260, -231.1115289952381033 ) ) ;
#20184 = CARTESIAN_POINT ( 'NONE',  ( 6.685304925496912354, 17.61973327427626046, -230.4152170797364931 ) ) ;
#20185 = CARTESIAN_POINT ( 'NONE',  ( -16.20072894238734307, 0.5024448614660336210, -230.4554067149722130 ) ) ;
#20186 = CARTESIAN_POINT ( 'NONE',  ( -13.84508897751235246, 5.904954704487344941, -218.7722818424232401 ) ) ;
#20187 = CARTESIAN_POINT ( 'NONE',  ( -14.78201816772319077, -5.155518158621814173, -222.1275223803717154 ) ) ;
#20188 = ORIENTED_EDGE ( 'NONE', *, *, #17171, .T. ) ;
#20189 = CONICAL_SURFACE ( 'NONE', #16263, 23.06814834742187514, 0.2617993877991500740 ) ;
#20190 = CARTESIAN_POINT ( 'NONE',  ( -9.810154340578240095, 25.84808829058669488, -220.5759521898573610 ) ) ;
#20191 = CARTESIAN_POINT ( 'NONE',  ( 17.66525298603349370, 4.919957226727790456, -233.3736646485340032 ) ) ;
#20192 = CARTESIAN_POINT ( 'NONE',  ( 9.400341091271927851, 28.64465517894215196, -231.0823126271420165 ) ) ;
#20193 = CARTESIAN_POINT ( 'NONE',  ( 27.76845665997775114, -9.103683020204879739, -229.9743915588940979 ) ) ;
#20194 = DIRECTION ( 'NONE',  ( 0.000000000000000000, 0.000000000000000000, 1.000000000000000000 ) ) ;
#20195 = ORIENTED_EDGE ( 'NONE', *, *, #14186, .F. ) ;
#20196 = CARTESIAN_POINT ( 'NONE',  ( -27.29953305526601426, 11.21644211419729054, -229.3676346105362995 ) ) ;
#20197 = CARTESIAN_POINT ( 'NONE',  ( -13.08850661186922260, -6.354795836388488439, -231.9371199848366984 ) ) ;
#20198 = DIRECTION ( 'NONE',  ( 0.000000000000000000, -0.7999999999999999334, -0.5999999999999999778 ) ) ;
#20199 = CARTESIAN_POINT ( 'NONE',  ( 4.559463107227270662, 13.27337529356814017, -226.9596205199204633 ) ) ;
#20200 = UNCERTAINTY_MEASURE_WITH_UNIT (LENGTH_MEASURE( 1.000000000000000082E-05 ), #12296, 'distance_accuracy_value', 'NONE');
#20201 = CARTESIAN_POINT ( 'NONE',  ( 8.818493748348606331, -10.89961555176610375, -227.9481955143288303 ) ) ;
#20202 = SURFACE_STYLE_FILL_AREA ( #21901 ) ;
#20203 = CARTESIAN_POINT ( 'NONE',  ( -15.15434969228324924, 4.423874646950748613, -230.6144467931089821 ) ) ;
#20204 = CARTESIAN_POINT ( 'NONE',  ( -18.63458318964815774, 8.046101765467303935, -217.8151248213926863 ) ) ;
#20205 = AXIS2_PLACEMENT_3D ( 'NONE', #7519, #14387, #21220 ) ;
#20206 = CARTESIAN_POINT ( 'NONE',  ( 25.70381634773192658, 10.55338509461953400, -230.3576492130207782 ) ) ;
#20207 = AXIS2_PLACEMENT_3D ( 'NONE', #12767, #5775, #20859 ) ;
#20208 = CARTESIAN_POINT ( 'NONE',  ( -21.00000000000000000, 0.000000000000000000, -75.00000000000000000 ) ) ;
#20209 = CARTESIAN_POINT ( 'NONE',  ( 18.76166303929371537, -3.000000000000002665, -225.0000000000001990 ) ) ;
#20210 = CARTESIAN_POINT ( 'NONE',  ( -1.232595164407830946E-29, 17.50000000000007105, -60.00000000000000000 ) ) ;
#20211 = CARTESIAN_POINT ( 'NONE',  ( -25.17982544627478703, 0.9072515815786372784, -215.5253307415545692 ) ) ;
#20212 = CARTESIAN_POINT ( 'NONE',  ( -13.67406442719345883, -9.319000780081536206, -231.1492214949047934 ) ) ;
#20213 = DIRECTION ( 'NONE',  ( 1.000000000000000000, 0.000000000000000000, 0.000000000000000000 ) ) ;
#20214 = CARTESIAN_POINT ( 'NONE',  ( 18.00000000000000000, 1.360023205165816762E-13, 0.000000000000000000 ) ) ;
#20215 = CARTESIAN_POINT ( 'NONE',  ( 4.936777854427027989, 27.97379167488809060, -227.0886654730259124 ) ) ;
#20216 = CARTESIAN_POINT ( 'NONE',  ( 7.898002370961310525, -21.57266348603731387, -216.1546105971396798 ) ) ;
#20217 = CARTESIAN_POINT ( 'NONE',  ( 10.40291689048662782, -13.87512507945592333, -231.9656913702303029 ) ) ;
#20218 = CARTESIAN_POINT ( 'NONE',  ( -16.50467377682197423, 21.56569464670658220, -229.9175202103629374 ) ) ;
#20219 = CARTESIAN_POINT ( 'NONE',  ( 25.50289296650958448, 5.998088869914441901, -233.1161630295026157 ) ) ;
#20220 = CARTESIAN_POINT ( 'NONE',  ( 15.99247752609008444, 10.72268246046808216, -230.5614800526110173 ) ) ;
#20221 = ORIENTED_EDGE ( 'NONE', *, *, #12275, .F. ) ;
#20222 = CARTESIAN_POINT ( 'NONE',  ( -12.75670220164522384, -23.12103459569904373, -229.1084755445707799 ) ) ;
#20223 = CARTESIAN_POINT ( 'NONE',  ( 1.526556658859590748E-13, -21.00000000000006395, 75.00000000000000000 ) ) ;
#20224 = CIRCLE ( 'NONE', #16648, 3.000000000000002665 ) ;
#20225 = CARTESIAN_POINT ( 'NONE',  ( -11.79271689233719478, 3.876813423829604144, -228.6816298097564299 ) ) ;
#20226 = AXIS2_PLACEMENT_3D ( 'NONE', #14730, #21682, #16632 ) ;
#20227 = CARTESIAN_POINT ( 'NONE',  ( 16.11883106748507188, 21.48229216499086291, -233.4985352728212433 ) ) ;
#20228 = CARTESIAN_POINT ( 'NONE',  ( 29.34815638429084927, -3.655059647784748122, -228.0165508611016207 ) ) ;
#20229 = CARTESIAN_POINT ( 'NONE',  ( 12.10245006109274080, 26.02147364279441888, -220.6079829738538649 ) ) ;
#20230 = CARTESIAN_POINT ( 'NONE',  ( -11.67631226053870996, 6.737291529340801333, -227.3110382950315227 ) ) ;
#20231 = ADVANCED_FACE ( 'NONE', ( #20000 ), #10523, .T. ) ;
#20232 = CARTESIAN_POINT ( 'NONE',  ( 17.60070748514786132, 25.68479983175475567, -229.9331108608050158 ) ) ;
#20233 = CARTESIAN_POINT ( 'NONE',  ( -25.06333669508177309, 2.553070212212491530, -230.2963116797556893 ) ) ;
#20234 = CARTESIAN_POINT ( 'NONE',  ( -4.104500432947460808, 15.73223271406093460, -218.0734292856946297 ) ) ;
#20235 = CARTESIAN_POINT ( 'NONE',  ( 7.744474050657649045, 7.483908733559392346, 92.00000000000000000 ) ) ;
#20236 = VECTOR ( 'NONE', #13851, 1000.000000000000000 ) ;
#20237 = CARTESIAN_POINT ( 'NONE',  ( 3.614175329767659761, 21.98488100320606264, -219.0898850257099753 ) ) ;
#20238 = AXIS2_PLACEMENT_3D ( 'NONE', #2315, #15952, #21212 ) ;
#20239 = CARTESIAN_POINT ( 'NONE',  ( 28.22932473237819551, -8.039268142081398949, -226.6539694142420558 ) ) ;
#20240 = CARTESIAN_POINT ( 'NONE',  ( -3.400000000000003908, 0.000000000000000000, -224.9999999999999716 ) ) ;
#20241 = CARTESIAN_POINT ( 'NONE',  ( -28.46519324992292965, -8.397260794665152517, -225.6705986409035347 ) ) ;
#20242 = CARTESIAN_POINT ( 'NONE',  ( -13.56011990957801139, -0.3895158544032599202, -219.3211261236655218 ) ) ;
#20243 = CARTESIAN_POINT ( 'NONE',  ( -13.72723917162997154, -9.146515947596070006, -227.8820830806802746 ) ) ;
#20244 = CARTESIAN_POINT ( 'NONE',  ( 18.76166303929371537, -3.000000000000002665, -225.0000000000001990 ) ) ;
#20245 = CARTESIAN_POINT ( 'NONE',  ( -4.170472558179216804, 16.67407401355319152, -230.2690496885289804 ) ) ;
#20246 = CARTESIAN_POINT ( 'NONE',  ( 6.930886114109415352, -28.33506752827666020, -226.0544877841801110 ) ) ;
#20247 = CARTESIAN_POINT ( 'NONE',  ( 19.70286159681817750, 17.87637900817293612, -218.6154571368943493 ) ) ;
#20248 = CARTESIAN_POINT ( 'NONE',  ( -4.855966894080006035, 26.75753167227873064, -230.1547293463117114 ) ) ;
#20249 = CARTESIAN_POINT ( 'NONE',  ( -7.329856113536736828, 10.17606210583481818, -226.3085553030691415 ) ) ;
#20250 = EDGE_LOOP ( 'NONE', ( #16100, #19452, #19862, #4456 ) ) ;
#20251 = CARTESIAN_POINT ( 'NONE',  ( -27.33303184979533285, -3.055344081261842870, -227.4850045670461043 ) ) ;
#20252 = CARTESIAN_POINT ( 'NONE',  ( 17.68508104102419409, 23.41266195669770767, -227.5327139115408954 ) ) ;
#20253 = CARTESIAN_POINT ( 'NONE',  ( -28.05279008194460744, 4.018900919424986284, -224.6698354068587662 ) ) ;
#20254 = DIRECTION ( 'NONE',  ( -1.000000000000000000, 0.000000000000000000, 0.000000000000000000 ) ) ;
#20255 = CARTESIAN_POINT ( 'NONE',  ( -28.96081738894762125, -0.4213479615504204800, -230.3891733152809707 ) ) ;
#20256 = CARTESIAN_POINT ( 'NONE',  ( 8.379126514044342500, 15.76264856365358646, -232.1787896114811360 ) ) ;
#20257 = CIRCLE ( 'NONE', #1228, 3.000000000000002665 ) ;
#20258 = CARTESIAN_POINT ( 'NONE',  ( -16.58624905143161143, 8.715293938925766426, -220.0618460037763384 ) ) ;
#20259 = CARTESIAN_POINT ( 'NONE',  ( -1.806671251568986669, 13.52068930966770388, -228.3567401718105430 ) ) ;
#20260 = CARTESIAN_POINT ( 'NONE',  ( 16.71272566993619080, 8.989703107375911273, -217.4612081447889125 ) ) ;
#20261 = EDGE_LOOP ( 'NONE', ( #20446, #21247, #3706, #7810, #10073, #7850 ) ) ;
#20262 = CARTESIAN_POINT ( 'NONE',  ( -20.07469464351956390, -22.83895492621963896, -220.1373730632280967 ) ) ;
#20263 = ORIENTED_EDGE ( 'NONE', *, *, #15829, .F. ) ;
#20264 = CARTESIAN_POINT ( 'NONE',  ( -7.786003226018990198, -12.23758553950863082, -224.1954257758910671 ) ) ;
#20265 = ADVANCED_FACE ( 'NONE', ( #3005 ), #13154, .F. ) ;
#20266 = CARTESIAN_POINT ( 'NONE',  ( -13.06407726305387307, 3.888674610242962348, -219.0371145420960204 ) ) ;
#20267 = CARTESIAN_POINT ( 'NONE',  ( 6.166782020495575445, -26.61202787628535660, -217.6604608484729795 ) ) ;
#20268 = CARTESIAN_POINT ( 'NONE',  ( 12.70896864779121316, -3.955665148817821386, -221.1719243096075900 ) ) ;
#20269 = CARTESIAN_POINT ( 'NONE',  ( -25.98129645912436914, -15.13773040547512139, -224.1390156429105787 ) ) ;
#20270 = CARTESIAN_POINT ( 'NONE',  ( 15.15306935214909778, 7.771180183537883757, -217.5526096523957165 ) ) ;
#20271 =( LENGTH_UNIT ( ) NAMED_UNIT ( * ) SI_UNIT ( .MILLI., .METRE. ) );
#20272 = CARTESIAN_POINT ( 'NONE',  ( -11.11479000491124047, 20.76372272540567110, -218.2001872134434564 ) ) ;
#20273 = CARTESIAN_POINT ( 'NONE',  ( 10.97349919442152810, 9.416813005082010690, -227.3764328406868742 ) ) ;
#20274 = AXIS2_PLACEMENT_3D ( 'NONE', #21712, #13284, #14351 ) ;
#20275 = CARTESIAN_POINT ( 'NONE',  ( 22.84140515590350518, 18.29101041979067332, -226.2334522600520472 ) ) ;
#20276 = CARTESIAN_POINT ( 'NONE',  ( 10.25308675723727347, 13.16459519580956972, -229.3963488176951273 ) ) ;
#20277 = CARTESIAN_POINT ( 'NONE',  ( 20.49803729918260942, -22.47924998572259980, -218.9346008044765028 ) ) ;
#20278 = CARTESIAN_POINT ( 'NONE',  ( -6.127117917506272882, 18.94558806480136681, -232.9763641438055117 ) ) ;
#20279 = CARTESIAN_POINT ( 'NONE',  ( -17.84981083811007707, 0.8485253248287054628, -231.8041300026935119 ) ) ;
#20280 = DIRECTION ( 'NONE',  ( 0.000000000000000000, 0.000000000000000000, -1.000000000000000000 ) ) ;
#20281 = CARTESIAN_POINT ( 'NONE',  ( 21.35706335192880445, 15.67286272432725092, -219.2578158352350783 ) ) ;
#20282 = CARTESIAN_POINT ( 'NONE',  ( 3.810076078852552950, -13.18001539772800612, -226.2402971015400510 ) ) ;
#20283 = CARTESIAN_POINT ( 'NONE',  ( -14.69827142695382527, 14.49176359921644597, -217.9600391472806109 ) ) ;
#20284 = CARTESIAN_POINT ( 'NONE',  ( -0.3197916200495275474, 16.38897215927557482, -229.9606066735827028 ) ) ;
#20285 = CARTESIAN_POINT ( 'NONE',  ( -11.49803752765619258, -8.459563989871591971, -222.4296168992866853 ) ) ;
#20286 = CARTESIAN_POINT ( 'NONE',  ( -27.28038240442402440, 5.683827137705129040, -226.0726697751923382 ) ) ;
#20288 = CARTESIAN_POINT ( 'NONE',  ( 24.34047711160105720, 17.90454708687460794, -228.1939002122307159 ) ) ;
#20287 = AXIS2_PLACEMENT_3D ( 'NONE', #4354, #18109, #5833 ) ;
#20289 = EDGE_LOOP ( 'NONE', ( #2624, #19099 ) ) ;
#20290 = CARTESIAN_POINT ( 'NONE',  ( -3.755296588130283553, 23.77975947300719284, -233.7323173085780752 ) ) ;
#20291 = CARTESIAN_POINT ( 'NONE',  ( 15.74534598441689504, -4.714293076379259873, -220.2687296774407173 ) ) ;
#20292 = CARTESIAN_POINT ( 'NONE',  ( 21.28562020585086501, -15.94148943779260819, -218.1725164024425396 ) ) ;
#20293 = LINE ( 'NONE', #18298, #19198 ) ;
#20294 = CARTESIAN_POINT ( 'NONE',  ( -2.808235066048971440, 30.42019778760651150, -222.6481917607299295 ) ) ;
#20295 = CARTESIAN_POINT ( 'NONE',  ( -19.75796449794633602, -18.82837501718038453, -216.0857152239166794 ) ) ;
#20296 = CARTESIAN_POINT ( 'NONE',  ( -8.803769170443210612, -17.82266517633203406, -233.6972128408098683 ) ) ;
#20297 = CARTESIAN_POINT ( 'NONE',  ( 20.38902395782249144, -18.95772103455488633, -230.9098670703349967 ) ) ;
#20298 = CARTESIAN_POINT ( 'NONE',  ( -8.137644474477026435, 12.10064032984799098, -226.6735072060122036 ) ) ;
#20299 = CARTESIAN_POINT ( 'NONE',  ( 11.16964468591631920, 25.71443501674299981, -224.7497461878887464 ) ) ;
#20300 = CARTESIAN_POINT ( 'NONE',  ( -16.74550766701807447, 3.787526820511904813, -217.9802846976114381 ) ) ;
#20301 = CARTESIAN_POINT ( 'NONE',  ( -14.64425879132321384, 10.88727730234500868, -217.2315376225554644 ) ) ;
#20302 = CARTESIAN_POINT ( 'NONE',  ( -17.87876569233342749, -13.82805272504658944, -230.9569051913176168 ) ) ;
#20303 = CARTESIAN_POINT ( 'NONE',  ( -10.32994309255856535, 16.55762392127841665, -218.3313395458419279 ) ) ;
#20304 = CARTESIAN_POINT ( 'NONE',  ( 15.26539804565921621, 9.309431686815628382, -232.9129599938668207 ) ) ;
#20305 = CARTESIAN_POINT ( 'NONE',  ( 8.126072675580726212, 14.68573014611672534, -233.8823376361746966 ) ) ;
#20306 = CARTESIAN_POINT ( 'NONE',  ( 14.41459438711767760, -7.262430563887544821, -219.0449948566021021 ) ) ;
#20307 = DIRECTION ( 'NONE',  ( 1.000000000000000000, 0.000000000000000000, 0.000000000000000000 ) ) ;
#20308 = ORIENTED_EDGE ( 'NONE', *, *, #19426, .F. ) ;
#20309 = CIRCLE ( 'NONE', #10630, 3.000000000000002665 ) ;
#20310 = CARTESIAN_POINT ( 'NONE',  ( -17.75316132689678383, 25.03468689048078843, -222.1645193425721061 ) ) ;
#20311 = CARTESIAN_POINT ( 'NONE',  ( -13.44328839870790837, -7.440897691988615392, -217.2299511873609106 ) ) ;
#20312 = PRODUCT_RELATED_PRODUCT_CATEGORY ( 'part', '', ( #6909 ) ) ;
#20313 = DIRECTION ( 'NONE',  ( 0.000000000000000000, 1.000000000000000000, -0.000000000000000000 ) ) ;
#20314 = CARTESIAN_POINT ( 'NONE',  ( 16.54345861550681107, 19.37554510112122230, -218.2240151908141002 ) ) ;
#20315 = FACE_OUTER_BOUND ( 'NONE', #16570, .T. ) ;
#20316 = CARTESIAN_POINT ( 'NONE',  ( 17.02763684969102798, -14.67205317233652195, -233.2001291093645818 ) ) ;
#20317 = CARTESIAN_POINT ( 'NONE',  ( -15.15110768032078070, 3.517015312212880218, -219.5479300368539270 ) ) ;
#20318 = CARTESIAN_POINT ( 'NONE',  ( -11.27928845652762213, 14.86256579634383002, -216.2427993537644966 ) ) ;
#20319 = CARTESIAN_POINT ( 'NONE',  ( 27.50364976068844669, 3.973406265104437729, -228.8805639113908228 ) ) ;
#20320 = CARTESIAN_POINT ( 'NONE',  ( -10.73077095140340376, -23.14408218571897891, -231.4559151628563995 ) ) ;
#20321 = CARTESIAN_POINT ( 'NONE',  ( -2.000000000000000000, 2.449293598294706414E-16, -105.0000000000000142 ) ) ;
#20322 = CARTESIAN_POINT ( 'NONE',  ( 15.52719855059926424, 1.633696074270991172, -221.7349885876216433 ) ) ;
#20323 = DIRECTION ( 'NONE',  ( -1.000000000000000000, 0.000000000000000000, 0.000000000000000000 ) ) ;
#20324 = CARTESIAN_POINT ( 'NONE',  ( 14.07866085257239419, -11.11077054092157645, -229.4139412770749971 ) ) ;
#20325 = STYLED_ITEM ( 'NONE', ( #314 ), #6798 ) ;
#20326 = CARTESIAN_POINT ( 'NONE',  ( 12.96537118559348478, -2.410286924380323104, -226.7941485364539460 ) ) ;
#20327 = MECHANICAL_DESIGN_GEOMETRIC_PRESENTATION_REPRESENTATION (  '', ( #14611 ), #16399 ) ;
#20328 = CARTESIAN_POINT ( 'NONE',  ( 21.91438441781873081, -0.08560050869741445134, -228.0000000000000000 ) ) ;
#20329 = CARTESIAN_POINT ( 'NONE',  ( 2.085064686336211892, 14.99578618537741548, -226.0985834012817861 ) ) ;
#20330 = CARTESIAN_POINT ( 'NONE',  ( 6.065954396161110651, -11.55577711821250553, -228.1182208427093485 ) ) ;
#20331 = CARTESIAN_POINT ( 'NONE',  ( 8.818493748348606331, -10.89961555176610375, -227.9481955143288303 ) ) ;
#20332 = ORIENTED_EDGE ( 'NONE', *, *, #5326, .T. ) ;
#20333 = CARTESIAN_POINT ( 'NONE',  ( -21.66803296057637951, 19.04503900041684616, -222.6603677762044526 ) ) ;
#20334 = CARTESIAN_POINT ( 'NONE',  ( 20.76808360334631232, 5.412616674732960931, -234.1222385626545304 ) ) ;
#20335 = CARTESIAN_POINT ( 'NONE',  ( 15.33128967029630729, 6.504525012335983902, -229.0514072561169883 ) ) ;
#20336 = ORIENTED_EDGE ( 'NONE', *, *, #18574, .T. ) ;
#20337 = CARTESIAN_POINT ( 'NONE',  ( -8.370291489323296474, -27.15533861588617981, -226.3382906634514597 ) ) ;
#20338 = CARTESIAN_POINT ( 'NONE',  ( -2.476137110235820948, -10.55034688490274242, 92.00000000000001421 ) ) ;
#20339 = CARTESIAN_POINT ( 'NONE',  ( -12.13319425917249283, 4.024026700415168634, -229.5243363405849095 ) ) ;
#20340 = CARTESIAN_POINT ( 'NONE',  ( 14.02309809840729393, 19.05079204846204277, -234.6885355850075143 ) ) ;
#20341 = CARTESIAN_POINT ( 'NONE',  ( 10.22171596740309418, -15.66339630224980972, -229.7686180632486810 ) ) ;
#20342 = CARTESIAN_POINT ( 'NONE',  ( 4.656903975822286768, 13.45000048768594780, -227.6722060245555497 ) ) ;
#20343 = CARTESIAN_POINT ( 'NONE',  ( -23.49379658590067876, 11.46840048879614393, -217.2519070826072323 ) ) ;
#20344 = CIRCLE ( 'NONE', #950, 23.00000000000008882 ) ;
#20345 = CARTESIAN_POINT ( 'NONE',  ( 9.400341091271927851, 28.64465517894215196, -231.0823126271420165 ) ) ;
#20346 = CARTESIAN_POINT ( 'NONE',  ( -17.00265675087485917, 7.324244386240115645, -218.5600005870616656 ) ) ;
#20347 = PRODUCT_DEFINITION_FORMATION_WITH_SPECIFIED_SOURCE ( 'ANY', '', #20542, .NOT_KNOWN. ) ;
#20348 = CARTESIAN_POINT ( 'NONE',  ( -5.807479211365208727, 19.77444019604324410, -216.0778658752277863 ) ) ;
#20349 = CARTESIAN_POINT ( 'NONE',  ( 16.91879448796214191, 0.8271603773820436212, -230.0510230802265710 ) ) ;
#20350 = CARTESIAN_POINT ( 'NONE',  ( 2.098184199980985376, -13.29281380427311099, -222.1652846463370281 ) ) ;
#20351 = CARTESIAN_POINT ( 'NONE',  ( 29.12543877365354916, -1.475122899492763873, -224.0746120762670444 ) ) ;
#20352 = CARTESIAN_POINT ( 'NONE',  ( -23.00000000000000000, -1.421401133463427911E-20, 10.00000000000000000 ) ) ;
#20353 = PRODUCT_DEFINITION_SHAPE ( 'NONE', 'NONE',  #16346 ) ;
#20354 = CARTESIAN_POINT ( 'NONE',  ( 2.465190328815661892E-29, 25.00000000000012790, 75.00000000000000000 ) ) ;
#20355 = CARTESIAN_POINT ( 'NONE',  ( 22.03647168420945590, 0.3315607655625663064, -232.0572713672586644 ) ) ;
#20356 = CARTESIAN_POINT ( 'NONE',  ( -10.33268794075157082, -17.24452578398873115, -232.5240627438851959 ) ) ;
#20357 = LINE ( 'NONE', #6648, #4175 ) ;
#20358 = EDGE_CURVE ( 'NONE', #16402, #3040, #8735, .T. ) ;
#20359 = SURFACE_STYLE_FILL_AREA ( #20582 ) ;
#20360 = CARTESIAN_POINT ( 'NONE',  ( 6.260833139380572732, -16.02228513277848876, -219.5457089733663736 ) ) ;
#20361 = CARTESIAN_POINT ( 'NONE',  ( 10.59524789654300925, 9.532374763983630928, -223.0758647391057821 ) ) ;
#20362 = CARTESIAN_POINT ( 'NONE',  ( -4.715783688792956063, 28.29821729825949816, -228.0423900005874600 ) ) ;
#20363 = CARTESIAN_POINT ( 'NONE',  ( -4.813101935419741295, 13.68373293383429434, -229.7840611589179503 ) ) ;
#20364 = VERTEX_POINT ( 'NONE', #1442 ) ;
#20365 = CARTESIAN_POINT ( 'NONE',  ( -21.86011749369748713, -1.271659148212478385, -218.8339345395071689 ) ) ;
#20366 = VERTEX_POINT ( 'NONE', #9774 ) ;
#20367 = CARTESIAN_POINT ( 'NONE',  ( 15.12287735332712835, 21.03907941686458116, -231.7894952627153202 ) ) ;
#20368 = CARTESIAN_POINT ( 'NONE',  ( 21.75737151495493649, -2.205713500382455283, -233.2756072794337285 ) ) ;
#20369 = CARTESIAN_POINT ( 'NONE',  ( 20.92846067405557520, -2.114533307883533109, -233.2756072794335580 ) ) ;
#20370 = DIRECTION ( 'NONE',  ( 0.000000000000000000, 0.000000000000000000, -1.000000000000000000 ) ) ;
#20371 = CARTESIAN_POINT ( 'NONE',  ( -13.00301829581513857, -0.4478114825397079279, -224.9470972339195214 ) ) ;
#20372 = CARTESIAN_POINT ( 'NONE',  ( 23.44028133050380802, 19.87677100428751231, -223.1503774981096342 ) ) ;
#20373 = CARTESIAN_POINT ( 'NONE',  ( -23.77327857871830830, 11.53128597905896768, -221.0855018166512025 ) ) ;
#20374 = CARTESIAN_POINT ( 'NONE',  ( 9.986779374595107228, 29.47523823012521049, -229.5287702428778687 ) ) ;
#20375 = CARTESIAN_POINT ( 'NONE',  ( 23.64727379217503866, 9.907944788639682088, -232.0643337313508709 ) ) ;
#20376 = CARTESIAN_POINT ( 'NONE',  ( -14.84991717770350661, -12.66914290363892270, -234.6513150936106626 ) ) ;
#20377 = EDGE_LOOP ( 'NONE', ( #9507, #9305, #21582, #18403 ) ) ;
#20378 = CARTESIAN_POINT ( 'NONE',  ( -12.60959727102843786, -12.64039607560028600, -218.2377899390859284 ) ) ;
#20379 = CARTESIAN_POINT ( 'NONE',  ( -19.86079186537285324, -0.7838168488858909821, -215.1601656726509475 ) ) ;
#20380 = CARTESIAN_POINT ( 'NONE',  ( 9.584731462935641488, -12.36622837314704348, -230.4796538097028531 ) ) ;
#20381 = CARTESIAN_POINT ( 'NONE',  ( 0.2389779871941385414, 16.64595486589868045, -218.1658233406367629 ) ) ;
#20382 = CARTESIAN_POINT ( 'NONE',  ( 30.29962988386644085, -7.724198041227372080, -225.2151988352147782 ) ) ;
#20383 = CARTESIAN_POINT ( 'NONE',  ( -27.88251101234890328, -7.575382714962081820, -221.6715981084135478 ) ) ;
#20384 = EDGE_CURVE ( 'NONE', #19977, #21087, #21281, .T. ) ;
#20385 = CARTESIAN_POINT ( 'NONE',  ( 10.14297843322460402, 14.69845403004500639, -219.2805000163441207 ) ) ;
#20386 = DIRECTION ( 'NONE',  ( 0.000000000000000000, 0.000000000000000000, -1.000000000000000000 ) ) ;
#20387 = CARTESIAN_POINT ( 'NONE',  ( -20.80338291456855870, 18.97067006663518995, -230.9007617602332516 ) ) ;
#20388 = CARTESIAN_POINT ( 'NONE',  ( 13.17768061945195157, 6.810183613937965674, -219.8302315341053657 ) ) ;
#20389 = CARTESIAN_POINT ( 'NONE',  ( 9.107417252317809186, 16.30291009569977234, -218.0131178633739921 ) ) ;
#20390 = CARTESIAN_POINT ( 'NONE',  ( 6.608541902967795423, 16.43938546752961116, -220.2982508316308952 ) ) ;
#20391 = CARTESIAN_POINT ( 'NONE',  ( 0.1236778125412633655, -13.14499247612405775, -221.8775184276742323 ) ) ;
#20392 = CARTESIAN_POINT ( 'NONE',  ( -5.762781846020777365, 12.94769902409342777, -223.1319556069387886 ) ) ;
#20393 = CARTESIAN_POINT ( 'NONE',  ( -13.98136146596813845, 3.850743984385103680, -228.7620665878280590 ) ) ;
#20394 = CARTESIAN_POINT ( 'NONE',  ( 0.000000000000000000, -23.00000000000000000, -75.00000000000000000 ) ) ;
#20395 = CARTESIAN_POINT ( 'NONE',  ( 18.06016678184731461, 2.257982981100609354, -218.9983079406065940 ) ) ;
#20396 = CARTESIAN_POINT ( 'NONE',  ( 3.489817674839083228, -23.52381883976217836, -233.5393804659674117 ) ) ;
#20397 = CARTESIAN_POINT ( 'NONE',  ( -20.71192633727912380, 6.339941255257877550, -217.2401662359725094 ) ) ;
#20398 = EDGE_CURVE ( 'NONE', #20089, #20147, #18960, .T. ) ;
#20399 = CARTESIAN_POINT ( 'NONE',  ( 3.219568897812384645, 28.82511222849302257, -221.5626884747494216 ) ) ;
#20400 = CARTESIAN_POINT ( 'NONE',  ( -15.27057301462635408, -17.00912219741827514, -233.6288396447818627 ) ) ;
#20401 = CARTESIAN_POINT ( 'NONE',  ( -27.32939371162572684, 5.861081283609568260, -224.9659309793921409 ) ) ;
#20402 = EDGE_CURVE ( 'NONE', #3651, #21555, #14490, .T. ) ;
#20403 = CARTESIAN_POINT ( 'NONE',  ( 7.174260007897984792, 9.971262771497068300, -226.2872513832048469 ) ) ;
#20404 = ORIENTED_EDGE ( 'NONE', *, *, #19866, .F. ) ;
#20405 = CARTESIAN_POINT ( 'NONE',  ( -4.104500432947460808, 15.73223271406093460, -218.0734292856946297 ) ) ;
#20406 = CARTESIAN_POINT ( 'NONE',  ( 14.29170853205465264, -5.149528714972483989, -227.7869631675187350 ) ) ;
#20407 = CARTESIAN_POINT ( 'NONE',  ( 19.19076252585518105, -11.68002947460017715, -233.4322573972352188 ) ) ;
#20408 = DIRECTION ( 'NONE',  ( 1.224646799147353207E-16, 1.000000000000000000, -0.000000000000000000 ) ) ;
#20409 = CARTESIAN_POINT ( 'NONE',  ( 11.82943521288609823, 27.58963564415041247, -226.1180395413371400 ) ) ;
#20410 = CARTESIAN_POINT ( 'NONE',  ( -21.59049550158629316, -10.60627468734379164, -215.2236992441505663 ) ) ;
#20411 = CARTESIAN_POINT ( 'NONE',  ( -7.832594822155400927, -23.57318293858060088, -216.4298491688572028 ) ) ;
#20412 = CARTESIAN_POINT ( 'NONE',  ( 11.31395536621571019, -8.070181239749643964, -225.0898076798974614 ) ) ;
#20413 = CARTESIAN_POINT ( 'NONE',  ( -14.01966324001334385, 10.60695606488527964, -217.6333332521996340 ) ) ;
#20414 = CARTESIAN_POINT ( 'NONE',  ( 10.64724148863252395, 12.28344647332184181, -223.6549461381946173 ) ) ;
#20415 = CARTESIAN_POINT ( 'NONE',  ( -18.70100282803782576, 16.58357028540773115, -216.4425743468854080 ) ) ;
#20416 = CARTESIAN_POINT ( 'NONE',  ( -10.76972226383489506, 9.682563335906554158, -229.2555443445334333 ) ) ;
#20417 = CARTESIAN_POINT ( 'NONE',  ( -15.91852731338648752, -4.625608912867816613, -229.2691880628015895 ) ) ;
#20418 = ORIENTED_EDGE ( 'NONE', *, *, #11174, .T. ) ;
#20419 = CARTESIAN_POINT ( 'NONE',  ( -14.94618804342693075, 22.09718979644185666, -219.6454806548149463 ) ) ;
#20420 = CARTESIAN_POINT ( 'NONE',  ( 17.29648694364601980, 10.20782262162153842, -233.8400727604031317 ) ) ;
#20421 = CARTESIAN_POINT ( 'NONE',  ( 13.79814099039094089, 16.09927043668092850, -214.6489469124405502 ) ) ;
#20422 = AXIS2_PLACEMENT_3D ( 'NONE', #20531, #13695, #10204 ) ;
#20423 = CARTESIAN_POINT ( 'NONE',  ( 23.27685575300125720, -16.81362096763192326, -220.1650456318757563 ) ) ;
#20425 = EDGE_CURVE ( 'NONE', #20853, #215, #4401, .T. ) ;
#20424 = DIRECTION ( 'NONE',  ( 0.000000000000000000, -1.000000000000000000, 0.000000000000000000 ) ) ;
#20426 = VERTEX_POINT ( 'NONE', #9888 ) ;
#20427 = CARTESIAN_POINT ( 'NONE',  ( -11.33137429837660193, 27.25022425932026238, -230.1650924901870212 ) ) ;
#20428 = CARTESIAN_POINT ( 'NONE',  ( -28.75820353979175081, -10.31764292692039753, -230.8958203355234389 ) ) ;
#20429 = DIRECTION ( 'NONE',  ( -0.000000000000000000, 0.000000000000000000, -1.000000000000000000 ) ) ;
#20430 = CARTESIAN_POINT ( 'NONE',  ( 24.58316096239279602, 5.861425670879941485, -231.3104446318280623 ) ) ;
#20431 = DIRECTION ( 'NONE',  ( 0.000000000000000000, 0.000000000000000000, -1.000000000000000000 ) ) ;
#20432 = CARTESIAN_POINT ( 'NONE',  ( 19.68037530048075112, -17.97179847169212508, -231.8517058357153076 ) ) ;
#20433 = CARTESIAN_POINT ( 'NONE',  ( -17.79285498209129202, 9.187865686019035749, -216.3798185811636756 ) ) ;
#20434 = CARTESIAN_POINT ( 'NONE',  ( 19.87150736056128864, 8.436445599727830924, -233.0166429845654932 ) ) ;
#20435 = CARTESIAN_POINT ( 'NONE',  ( -12.58820391453271093, -22.27128923838312247, -218.3899974299303324 ) ) ;
#20436 = CARTESIAN_POINT ( 'NONE',  ( 1.526556658859590243E-13, -22.63401512838748175, -77.51594804401857175 ) ) ;
#20437 = CARTESIAN_POINT ( 'NONE',  ( 21.65323058444409909, -0.3442074641359690323, -222.0185703855663348 ) ) ;
#20438 = CARTESIAN_POINT ( 'NONE',  ( -1.232595164407830946E-29, 17.50000000000007105, -55.00000000000000000 ) ) ;
#20439 = CARTESIAN_POINT ( 'NONE',  ( 15.27128302093890255, -22.10320814337061535, -229.9052109820655119 ) ) ;
#20440 = CARTESIAN_POINT ( 'NONE',  ( 12.90388673151985977, -2.516900468902075083, -226.6432736121070661 ) ) ;
#20441 = CARTESIAN_POINT ( 'NONE',  ( 20.62542899963628784, -1.332263963074644231, -227.6939020710331363 ) ) ;
#20442 = CARTESIAN_POINT ( 'NONE',  ( 12.91443243054181700, 13.28840485332751875, -229.6651346406987955 ) ) ;
#20443 = CARTESIAN_POINT ( 'NONE',  ( 5.066530254613678785, 15.76189963344335254, -222.1234037505291781 ) ) ;
#20444 = CARTESIAN_POINT ( 'NONE',  ( 8.679960083554519201, -14.04048791834972398, -217.5462328905347249 ) ) ;
#20445 = CARTESIAN_POINT ( 'NONE',  ( 17.02763684969102798, -14.67205317233652195, -233.2001291093645818 ) ) ;
#20446 = ORIENTED_EDGE ( 'NONE', *, *, #13126, .T. ) ;
#20447 = CARTESIAN_POINT ( 'NONE',  ( -7.464187997994982560, 14.20693289415472016, -228.8865298551900764 ) ) ;
#20448 = CARTESIAN_POINT ( 'NONE',  ( -18.42638600874552424, 7.060399206045774534, -230.3991437614443214 ) ) ;
#20449 = CARTESIAN_POINT ( 'NONE',  ( 14.18323607655884722, 3.286047475533308226, -222.8710065128477140 ) ) ;
#20450 = EDGE_LOOP ( 'NONE', ( #15033, #13640, #7962, #7218 ) ) ;
#20451 = CARTESIAN_POINT ( 'NONE',  ( -6.479026444546563290, -23.11309618162032820, -231.4158670874050756 ) ) ;
#20452 = PLANE ( 'NONE',  #20554 ) ;
#20453 = EDGE_LOOP ( 'NONE', ( #21958, #21874, #837, #17957 ) ) ;
#20454 = VERTEX_POINT ( 'NONE', #20105 ) ;
#20455 = CARTESIAN_POINT ( 'NONE',  ( 3.490829917597003895, 11.40812925993816229, -222.8973702487053004 ) ) ;
#20456 = CARTESIAN_POINT ( 'NONE',  ( 10.85678324124089755, -13.97331853324622131, -221.1336851750754420 ) ) ;
#20457 = CARTESIAN_POINT ( 'NONE',  ( 5.248230734842167955, 23.54336384919183445, -216.8914391693808739 ) ) ;
#20458 = CARTESIAN_POINT ( 'NONE',  ( -14.29986196492902550, 0.06805469746732484282, -227.4167624117703213 ) ) ;
#20459 = CARTESIAN_POINT ( 'NONE',  ( 9.168912942254459963, 16.03578711007639157, -234.6923200900793347 ) ) ;
#20460 = CARTESIAN_POINT ( 'NONE',  ( -14.58084844870496966, 13.85720943031455832, -233.3219724312919254 ) ) ;
#20461 = CARTESIAN_POINT ( 'NONE',  ( -3.855805549595750392, 26.68244055262801950, -232.4569730455296508 ) ) ;
#20462 = CARTESIAN_POINT ( 'NONE',  ( 22.00000000000000711, 0.000000000000000000, -233.0000000000000284 ) ) ;
#20463 = CARTESIAN_POINT ( 'NONE',  ( 1.292981098121811279, -26.53499626907933262, -232.9055005154886828 ) ) ;
#20464 = CARTESIAN_POINT ( 'NONE',  ( 16.50235023187294203, -3.000022380394500310, -230.0447763498268614 ) ) ;
#20465 = CARTESIAN_POINT ( 'NONE',  ( -25.00000000000000000, 3.214196380386082240E-15, 75.00000000000000000 ) ) ;
#20466 = CARTESIAN_POINT ( 'NONE',  ( 27.75679124201660741, 4.911524026080384075, -221.4430403652340829 ) ) ;
#20467 = CARTESIAN_POINT ( 'NONE',  ( -15.95469971785872332, -24.72796590591627464, -225.3946449442874211 ) ) ;
#20468 = DIRECTION ( 'NONE',  ( 1.000000000000000000, 0.000000000000000000, 0.000000000000000000 ) ) ;
#20469 = CARTESIAN_POINT ( 'NONE',  ( 6.755953262402430326, -28.44658494672641424, -224.7309905328439754 ) ) ;
#20470 = CARTESIAN_POINT ( 'NONE',  ( -18.05576253097465766, 2.935622250037499104, -232.1557308718028594 ) ) ;
#20471 = CARTESIAN_POINT ( 'NONE',  ( -3.996294969088721505, 28.80481464818193515, -222.8623509149411746 ) ) ;
#20472 = CARTESIAN_POINT ( 'NONE',  ( -22.56222084847001597, 18.89892770556097901, -231.8972396388394088 ) ) ;
#20473 = ORIENTED_EDGE ( 'NONE', *, *, #14777, .T. ) ;
#20474 = CARTESIAN_POINT ( 'NONE',  ( -26.74184309910812374, -3.166857098814535032, -228.4517881524372456 ) ) ;
#20475 = ORIENTED_EDGE ( 'NONE', *, *, #19953, .F. ) ;
#20476 = CARTESIAN_POINT ( 'NONE',  ( 11.57669841200422134, 10.63052136557218574, -228.9489978335593889 ) ) ;
#20477 = EDGE_CURVE ( 'NONE', #15308, #6745, #4693, .T. ) ;
#20478 = CARTESIAN_POINT ( 'NONE',  ( -24.05551141223569545, 2.266836731622281498, -230.7594878221277384 ) ) ;
#20479 = CARTESIAN_POINT ( 'NONE',  ( -24.53276002501160136, 17.12571705644413811, -226.2419685911331442 ) ) ;
#20480 = CARTESIAN_POINT ( 'NONE',  ( -3.400000000000003908, 0.000000000000000000, -227.9999999999999716 ) ) ;
#20481 = CARTESIAN_POINT ( 'NONE',  ( 5.833753951408669813, 12.47745132051510453, -226.2508980627489450 ) ) ;
#20482 = CARTESIAN_POINT ( 'NONE',  ( -15.82068653568960137, 8.372322471091806051, -220.7139663195713979 ) ) ;
#20483 = CARTESIAN_POINT ( 'NONE',  ( 7.283976506941576723, 24.82246917020504284, -234.3244871078919402 ) ) ;
#20484 = CARTESIAN_POINT ( 'NONE',  ( 18.78616100366561881, 3.045752412654093355, -231.5393376370170699 ) ) ;
#20485 = CARTESIAN_POINT ( 'NONE',  ( -9.899145469884247817, -15.57979392722981693, -233.4163339629578786 ) ) ;
#20486 = ORIENTED_EDGE ( 'NONE', *, *, #11762, .F. ) ;
#20487 = CARTESIAN_POINT ( 'NONE',  ( -13.55429797312971374, -24.97278848321653300, -221.1627755146857908 ) ) ;
#20488 = CARTESIAN_POINT ( 'NONE',  ( -14.00980274651940682, 20.05588230486321066, -234.2453272803952586 ) ) ;
#20489 = CARTESIAN_POINT ( 'NONE',  ( 1.799766247726228174, -14.75051420185460849, -230.6199496058247291 ) ) ;
#20490 = CARTESIAN_POINT ( 'NONE',  ( -7.429838964355703901, 14.87322129099639234, -232.2632863647814077 ) ) ;
#20491 = CARTESIAN_POINT ( 'NONE',  ( 25.51806929334465934, -15.64550748320022144, -218.8629450469393589 ) ) ;
#20492 = AXIS2_PLACEMENT_3D ( 'NONE', #7282, #20989, #12457 ) ;
#20493 = CARTESIAN_POINT ( 'NONE',  ( -15.15819830826754355, -2.370657588173597841, -221.8013720140894236 ) ) ;
#20494 = CARTESIAN_POINT ( 'NONE',  ( 11.17884645811568944, 10.10284797925214662, -221.0856722371208036 ) ) ;
#20495 = DIRECTION ( 'NONE',  ( 1.000000000000000000, 6.982962677686272233E-15, 0.000000000000000000 ) ) ;
#20496 = CARTESIAN_POINT ( 'NONE',  ( -6.901278853520646628, 15.41233971300566807, -220.5972764307651346 ) ) ;
#20497 = CARTESIAN_POINT ( 'NONE',  ( 26.72610819325501907, 14.97064052581051108, -224.6384473985499426 ) ) ;
#20498 = CARTESIAN_POINT ( 'NONE',  ( 13.03557269046774714, 7.519834803053426775, -226.9490612297269081 ) ) ;
#20499 = CARTESIAN_POINT ( 'NONE',  ( 23.08329078023534109, 11.96623404944238978, -217.1428499060670845 ) ) ;
#20500 = CARTESIAN_POINT ( 'NONE',  ( 0.2060740257213805326, -13.46849591350090947, -221.0879548523055860 ) ) ;
#20501 = CARTESIAN_POINT ( 'NONE',  ( -10.07004052286948337, 22.64471483900350179, -217.4645417110143626 ) ) ;
#20502 = CARTESIAN_POINT ( 'NONE',  ( 27.75679124201660741, 4.911524026080384075, -221.4430403652340829 ) ) ;
#20503 = CARTESIAN_POINT ( 'NONE',  ( 7.434033643350927534, -13.76500825175950027, -228.7793665183827159 ) ) ;
#20504 = CARTESIAN_POINT ( 'NONE',  ( -13.93825237094548619, 9.044872709574327985, -220.1275804576921757 ) ) ;
#20505 = CARTESIAN_POINT ( 'NONE',  ( 9.527502190795640757, 23.55559004943647139, -217.4101659741468211 ) ) ;
#20506 = ADVANCED_FACE ( 'NONE', ( #16754 ), #6501, .T. ) ;
#20507 = CARTESIAN_POINT ( 'NONE',  ( -23.84209965496292227, -7.976777114481962805, -232.1458837748831456 ) ) ;
#20508 = CONTEXT_DEPENDENT_SHAPE_REPRESENTATION ( #15630, #6728 ) ;
#20509 = CARTESIAN_POINT ( 'NONE',  ( -21.47149190714903710, 3.672831083387290363, -231.0833634068433469 ) ) ;
#20510 = CARTESIAN_POINT ( 'NONE',  ( 10.61539692146153691, 8.157890242340682718, -227.5705019877536301 ) ) ;
#20511 = EDGE_LOOP ( 'NONE', ( #8888, #15771, #5895, #17674 ) ) ;
#20512 = CARTESIAN_POINT ( 'NONE',  ( 17.19674704922021391, 23.07334190050143974, -228.8256488842130238 ) ) ;
#20513 = CARTESIAN_POINT ( 'NONE',  ( 20.48752708986941329, -13.44209471493726937, -230.9762584513030106 ) ) ;
#20514 = CARTESIAN_POINT ( 'NONE',  ( 11.81564506561547390, -6.597897255275705142, -225.1493936678799628 ) ) ;
#20515 = CARTESIAN_POINT ( 'NONE',  ( 15.85665641241444668, 18.24713744004561988, -217.7195292979064902 ) ) ;
#20516 = CARTESIAN_POINT ( 'NONE',  ( -26.70887854271809658, -5.532318215328999145, -217.2738835169348306 ) ) ;
#20517 = CARTESIAN_POINT ( 'NONE',  ( -8.257247207528708444, -26.39349301559143512, -217.9383130379005138 ) ) ;
#20518 = CARTESIAN_POINT ( 'NONE',  ( 5.569356713096689226, -12.06902110579006226, -223.1407905962607003 ) ) ;
#20519 = CARTESIAN_POINT ( 'NONE',  ( -17.07051451008491938, 15.19890664381897949, -233.6014043774825666 ) ) ;
#20520 = EDGE_CURVE ( 'NONE', #15223, #497, #20976, .T. ) ;
#20521 = CARTESIAN_POINT ( 'NONE',  ( 16.53859560591101641, 22.24348416270211359, -223.7250258089275974 ) ) ;
#20522 = CARTESIAN_POINT ( 'NONE',  ( -24.24202834850560606, 19.05981756344202438, -226.6980666352953335 ) ) ;
#20523 = CARTESIAN_POINT ( 'NONE',  ( -11.36937006530106586, 5.486019310970209339, -224.0742584078730033 ) ) ;
#20524 = CARTESIAN_POINT ( 'NONE',  ( 30.05917755080113096, -2.930701380670650114, -221.3976229872638726 ) ) ;
#20525 = VERTEX_POINT ( 'NONE', #17726 ) ;
#20526 = CIRCLE ( 'NONE', #16591, 17.50000000000000355 ) ;
#20527 = CARTESIAN_POINT ( 'NONE',  ( -3.996294969088721505, 28.80481464818193515, -222.8623509149411746 ) ) ;
#20528 = CARTESIAN_POINT ( 'NONE',  ( 29.11492790716816614, 6.132849117128307270, -229.8316941169402412 ) ) ;
#20529 = CARTESIAN_POINT ( 'NONE',  ( 8.681721411120292942, 8.442847255497570202, -228.0516816418615065 ) ) ;
#20530 = CARTESIAN_POINT ( 'NONE',  ( 14.46917091355089902, -8.493370822347547033, -231.7163745456035997 ) ) ;
#20531 = CARTESIAN_POINT ( 'NONE',  ( 0.000000000000000000, 0.000000000000000000, -99.99999999999998579 ) ) ;
#20532 = ORIENTED_EDGE ( 'NONE', *, *, #16914, .F. ) ;
#20533 = CARTESIAN_POINT ( 'NONE',  ( -10.24288955603410933, 28.30762631303078791, -220.8855665231519083 ) ) ;
#20534 = CARTESIAN_POINT ( 'NONE',  ( -13.37406041957185110, -11.77244451953823834, -233.9958171493936732 ) ) ;
#20535 = CARTESIAN_POINT ( 'NONE',  ( 25.50000000000000000, -0.5000000000000000000, 0.000000000000000000 ) ) ;
#20536 = VECTOR ( 'NONE', #3712, 1000.000000000000000 ) ;
#20537 = CARTESIAN_POINT ( 'NONE',  ( 18.04365516558436866, 6.721233635139160612, -218.4376093631473168 ) ) ;
#20538 = DIRECTION ( 'NONE',  ( 1.000000000000000000, 0.000000000000000000, 0.000000000000000000 ) ) ;
#20539 = CARTESIAN_POINT ( 'NONE',  ( 12.70477135646371281, -9.814387909761604689, -230.3443492180780652 ) ) ;
#20540 = SURFACE_STYLE_FILL_AREA ( #13704 ) ;
#20541 = CARTESIAN_POINT ( 'NONE',  ( -14.70651859537745487, 4.211702956367679107, -230.0357207626005334 ) ) ;
#20542 = PRODUCT ( 'motor', 'motor', '', ( #12673 ) ) ;
#20543 = CARTESIAN_POINT ( 'NONE',  ( -16.74550766701807447, 3.787526820511904813, -217.9802846976114381 ) ) ;
#20544 = CARTESIAN_POINT ( 'NONE',  ( -7.086613078029399659, -28.17108726511417771, -223.6412629831645233 ) ) ;
#20545 = VECTOR ( 'NONE', #5791, 1000.000000000000000 ) ;
#20546 = CARTESIAN_POINT ( 'NONE',  ( 0.000000000000000000, 0.000000000000000000, 93.00000000000000000 ) ) ;
#20547 = CARTESIAN_POINT ( 'NONE',  ( 0.000000000000000000, 19.80000000000006111, 78.50000000000000000 ) ) ;
#20548 = DIRECTION ( 'NONE',  ( -0.000000000000000000, 0.000000000000000000, -1.000000000000000000 ) ) ;
#20549 = CARTESIAN_POINT ( 'NONE',  ( 17.83206265427627457, -15.38023228143295640, -231.0294926223175480 ) ) ;
#20550 = CARTESIAN_POINT ( 'NONE',  ( 2.465190328815661892E-29, 24.63401512838760610, -77.51594804401857175 ) ) ;
#20551 = CARTESIAN_POINT ( 'NONE',  ( -22.85901844618171097, -2.626155446365975976, 9.672066817478860656 ) ) ;
#20552 = CARTESIAN_POINT ( 'NONE',  ( 17.35243190875273811, 16.67741344734974263, -230.5744436858935558 ) ) ;
#20553 = EDGE_CURVE ( 'NONE', #1152, #15384, #9388, .T. ) ;
#20554 = AXIS2_PLACEMENT_3D ( 'NONE', #5041, #3350, #2115 ) ;
#20555 = CARTESIAN_POINT ( 'NONE',  ( 5.791579991237209235, 15.48299465423324861, -228.0203551130359472 ) ) ;
#20556 = CARTESIAN_POINT ( 'NONE',  ( 6.644147376113458847, -12.60537238651543923, -230.3381876225809037 ) ) ;
#20557 = CARTESIAN_POINT ( 'NONE',  ( 5.569356713096689226, -12.06902110579006226, -223.1407905962607003 ) ) ;
#20558 = ORIENTED_EDGE ( 'NONE', *, *, #13692, .F. ) ;
#20559 = CARTESIAN_POINT ( 'NONE',  ( -9.233762381136051189, 19.18161952504991419, -232.0796851897838451 ) ) ;
#20560 = CARTESIAN_POINT ( 'NONE',  ( -25.17056316833229701, 11.10725809642625705, -227.0225660235207386 ) ) ;
#20561 = CARTESIAN_POINT ( 'NONE',  ( 20.41968681625622040, 10.18377600976054076, -218.1989382652844256 ) ) ;
#20562 = ORIENTED_EDGE ( 'NONE', *, *, #5532, .T. ) ;
#20563 = CARTESIAN_POINT ( 'NONE',  ( -3.088421015035204498, -25.33386621341791667, -218.8172537214380498 ) ) ;
#20564 = CARTESIAN_POINT ( 'NONE',  ( 0.000000000000000000, 0.000000000000000000, -30.00000000000000000 ) ) ;
#20565 = ORIENTED_EDGE ( 'NONE', *, *, #18365, .F. ) ;
#20566 = CARTESIAN_POINT ( 'NONE',  ( 27.08994772491946890, 9.675875910685000747, -221.3471992134593336 ) ) ;
#20567 = CARTESIAN_POINT ( 'NONE',  ( 11.82295278175540787, -22.41907685134884076, -220.1071383070178342 ) ) ;
#20568 = CARTESIAN_POINT ( 'NONE',  ( 11.33210854356620523, 22.81476816607802149, -217.8536224460118262 ) ) ;
#20569 = CARTESIAN_POINT ( 'NONE',  ( -6.855867220396999251, 12.17758473459128332, -220.6375607554995213 ) ) ;
#20570 = AXIS2_PLACEMENT_3D ( 'NONE', #6077, #2478, #19910 ) ;
#20571 = CARTESIAN_POINT ( 'NONE',  ( 28.41961022423218353, 10.76616830294286409, -220.2698681100053193 ) ) ;
#20572 = CARTESIAN_POINT ( 'NONE',  ( -4.620781219515533778, 16.99182040716223696, -217.1278208835672672 ) ) ;
#20573 = DIRECTION ( 'NONE',  ( -1.000000000000000000, 0.000000000000000000, 0.000000000000000000 ) ) ;
#20574 = CARTESIAN_POINT ( 'NONE',  ( 8.257114973007913861, -25.39836461225790742, -232.6217252414676295 ) ) ;
#20575 = CARTESIAN_POINT ( 'NONE',  ( 26.16486877413895584, -0.2437668799822691745, -230.8325409000573814 ) ) ;
#20576 = CARTESIAN_POINT ( 'NONE',  ( 2.999999999999975131, 3.673940397442065291E-16, -105.0000000000000142 ) ) ;
#20577 = CARTESIAN_POINT ( 'NONE',  ( -15.46216926290318305, -2.495270579625169738, -221.2150947962298631 ) ) ;
#20578 = CARTESIAN_POINT ( 'NONE',  ( 15.05360126642391450, 1.481754003466396963, -222.9454997252120734 ) ) ;
#20579 = CARTESIAN_POINT ( 'NONE',  ( -17.12341639776428437, -14.09197680242149886, -218.6048700820433339 ) ) ;
#20580 = CONICAL_SURFACE ( 'NONE', #10899, 23.06814834742187514, 0.2617993877991500740 ) ;
#20581 = AXIS2_PLACEMENT_3D ( 'NONE', #21464, #1105, #18001 ) ;
#20582 = FILL_AREA_STYLE ('',( #20131 ) ) ;
#20583 = CARTESIAN_POINT ( 'NONE',  ( 13.38323588254664642, -24.59169381177348157, -229.6955247737395780 ) ) ;
#20584 = CARTESIAN_POINT ( 'NONE',  ( 29.01678366425524658, 8.126504218505314014, -229.6975090854573125 ) ) ;
#20585 = CARTESIAN_POINT ( 'NONE',  ( 3.291078285693179950, 23.55624334554876498, -217.3208248278388623 ) ) ;
#20586 = CARTESIAN_POINT ( 'NONE',  ( -8.716816145717144693, 12.22834664005217675, -231.7124508691059646 ) ) ;
#20587 = ORIENTED_EDGE ( 'NONE', *, *, #15067, .F. ) ;
#20588 = CARTESIAN_POINT ( 'NONE',  ( 25.69869100782391413, -6.466588899411362057, -234.2905747065633193 ) ) ;
#20589 = EDGE_LOOP ( 'NONE', ( #13131, #17139, #14617, #20044 ) ) ;
#20590 = CARTESIAN_POINT ( 'NONE',  ( 12.23063869552301242, 12.84118223717021934, -218.8273164334868284 ) ) ;
#20591 = CARTESIAN_POINT ( 'NONE',  ( -23.43012680803641956, 15.46310457140252304, -230.0052977649806962 ) ) ;
#20592 = CARTESIAN_POINT ( 'NONE',  ( -23.43012680803641956, 15.46310457140252304, -230.0052977649806962 ) ) ;
#20593 = CARTESIAN_POINT ( 'NONE',  ( -8.652743106909156268, -19.89692808811530966, -232.3032230114403376 ) ) ;
#20594 = PLANE ( 'NONE',  #5853 ) ;
#20595 = CARTESIAN_POINT ( 'NONE',  ( 25.38325563848796662, 11.05100313887457553, -217.8685524735130628 ) ) ;
#20596 = CARTESIAN_POINT ( 'NONE',  ( -16.37512411505367282, 2.406627362596846620, -227.7341547288202719 ) ) ;
#20597 = AXIS2_PLACEMENT_3D ( 'NONE', #15297, #11566, #15182 ) ;
#20598 = CARTESIAN_POINT ( 'NONE',  ( 10.85325209735074559, 11.82487774067193342, -216.5214842375702062 ) ) ;
#20599 = CARTESIAN_POINT ( 'NONE',  ( 19.66580438618080251, 15.18147523775131624, -233.5153994334876586 ) ) ;
#20600 = CARTESIAN_POINT ( 'NONE',  ( -5.045022908720540045, -16.91549468467126616, -232.0765493255083243 ) ) ;
#20601 = ORIENTED_EDGE ( 'NONE', *, *, #21445, .T. ) ;
#20602 = CARTESIAN_POINT ( 'NONE',  ( -5.249799428260828904, -14.16826377401270065, -226.9124264195330056 ) ) ;
#20603 = ADVANCED_FACE ( 'NONE', ( #3978 ), #12325, .F. ) ;
#20604 = CARTESIAN_POINT ( 'NONE',  ( -11.87391433320165746, 8.920676825367966245, -232.2044275666449096 ) ) ;
#20605 = CARTESIAN_POINT ( 'NONE',  ( 15.60497028854143764, -26.39208911975253002, -225.8550158017044112 ) ) ;
#20606 = CARTESIAN_POINT ( 'NONE',  ( -3.326157069579807946, 13.92020081821418565, -220.5733722327383930 ) ) ;
#20607 = CARTESIAN_POINT ( 'NONE',  ( 12.64197975508134597, -4.295353707277522304, -228.6481500018833799 ) ) ;
#20608 = CARTESIAN_POINT ( 'NONE',  ( -25.61235545225478560, -15.41032726095661509, -226.9890212492312855 ) ) ;
#20609 = CARTESIAN_POINT ( 'NONE',  ( -27.52457542293397097, 5.447957517019466067, -230.2717933641555135 ) ) ;
#20610 =( NAMED_UNIT ( * ) PLANE_ANGLE_UNIT ( ) SI_UNIT ( $, .RADIAN. ) );
#20611 = CARTESIAN_POINT ( 'NONE',  ( -3.389634396460917465, 16.42708991135657115, -221.9057377485790994 ) ) ;
#20612 = CARTESIAN_POINT ( 'NONE',  ( -20.45797657813638182, 1.164962349958370336, -217.1306074022350572 ) ) ;
#20613 = CARTESIAN_POINT ( 'NONE',  ( 8.689059922489732912, 15.18271246186214363, -218.7354841152034908 ) ) ;
#20614 = CARTESIAN_POINT ( 'NONE',  ( 18.13412043358480474, 12.55378873098427128, -233.2186159706515696 ) ) ;
#20615 = CARTESIAN_POINT ( 'NONE',  ( 5.917072789534883803, -21.18442853552521754, -235.1867574136372525 ) ) ;
#20616 = AXIS2_PLACEMENT_3D ( 'NONE', #2779, #21460, #9556 ) ;
#20617 = CARTESIAN_POINT ( 'NONE',  ( 19.07698357483942786, 25.86742807064150895, -222.6991278896559834 ) ) ;
#20618 = AXIS2_PLACEMENT_3D ( 'NONE', #13484, #18876, #13710 ) ;
#20619 = PLANE ( 'NONE',  #17710 ) ;
#20620 = ADVANCED_BREP_SHAPE_REPRESENTATION ( '', ( #6837, #6677 ), #2013 ) ;
#20621 = CARTESIAN_POINT ( 'NONE',  ( 9.923594862512629788, -27.47695806889172943, -228.4416101659923015 ) ) ;
#20622 = CARTESIAN_POINT ( 'NONE',  ( -14.94618804342693075, 22.09718979644185666, -219.6454806548149463 ) ) ;
#20623 = CARTESIAN_POINT ( 'NONE',  ( 3.291078285693179950, 23.55624334554876498, -217.3208248278388623 ) ) ;
#20624 = CARTESIAN_POINT ( 'NONE',  ( -13.88883449434014672, -11.15328429608096172, -217.8357414694029046 ) ) ;
#20625 = CARTESIAN_POINT ( 'NONE',  ( -15.32935061426341861, 5.146212415319166844, -225.5669090095357774 ) ) ;
#20626 = CARTESIAN_POINT ( 'NONE',  ( 12.99334571784053338, 27.47142594410712846, -219.5003755906066658 ) ) ;
#20627 = CARTESIAN_POINT ( 'NONE',  ( 7.743212835174657194, 11.90778931056080481, -226.0491028376908105 ) ) ;
#20628 = CARTESIAN_POINT ( 'NONE',  ( 23.44453178257692727, -8.594063734448958769, -231.6993511358095361 ) ) ;
#20629 = ORIENTED_EDGE ( 'NONE', *, *, #10180, .F. ) ;
#20630 = CARTESIAN_POINT ( 'NONE',  ( 13.37423534347618670, -3.100899090186935325, -222.2483675785374260 ) ) ;
#20631 =( REPRESENTATION_RELATIONSHIP ('NONE','NONE', #5277, #8462 ) REPRESENTATION_RELATIONSHIP_WITH_TRANSFORMATION ( #13329 )SHAPE_REPRESENTATION_RELATIONSHIP( ) );
#20632 = DIRECTION ( 'NONE',  ( -1.000000000000000000, 0.000000000000000000, 0.000000000000000000 ) ) ;
#20633 = MECHANICAL_DESIGN_GEOMETRIC_PRESENTATION_REPRESENTATION (  '', ( #7000 ), #12399 ) ;
#20634 = CARTESIAN_POINT ( 'NONE',  ( 8.329997790135040603, 12.51216704542961899, -228.7022893680961602 ) ) ;
#20635 = CARTESIAN_POINT ( 'NONE',  ( -19.19980083083115474, -2.588899828715947038, -216.2953230342753557 ) ) ;
#20636 = CARTESIAN_POINT ( 'NONE',  ( -1.177898122437396333, -26.14463525305933445, -216.8677949074964033 ) ) ;
#20637 = CARTESIAN_POINT ( 'NONE',  ( 18.00123703865980218, -15.82960056198189491, -233.0014896689109776 ) ) ;
#20638 = CARTESIAN_POINT ( 'NONE',  ( -0.6272116608575281083, 20.18031380156121202, -219.3960054794027030 ) ) ;
#20639 = CARTESIAN_POINT ( 'NONE',  ( 0.000000000000000000, 0.000000000000000000, -55.00000000000000000 ) ) ;
#20640 = CARTESIAN_POINT ( 'NONE',  ( 14.40184562439531213, 6.414772937171507650, -227.4651811604036595 ) ) ;
#20641 = CARTESIAN_POINT ( 'NONE',  ( -11.49049084071896409, 11.06834963248926940, -218.3354249205727058 ) ) ;
#20642 = CARTESIAN_POINT ( 'NONE',  ( -5.600903697806950632, 21.62055466701630735, -218.6671277943675307 ) ) ;
#20643 = CARTESIAN_POINT ( 'NONE',  ( 14.79879825009101069, -3.130997509566451953, -219.4569190381675696 ) ) ;
#20644 = EDGE_CURVE ( 'NONE', #11119, #13087, #3333, .T. ) ;
#20645 = VERTEX_POINT ( 'NONE', #10749 ) ;
#20646 = CARTESIAN_POINT ( 'NONE',  ( -0.3197916200495275474, 16.38897215927557482, -229.9606066735827028 ) ) ;
#20647 = CARTESIAN_POINT ( 'NONE',  ( -16.03353370602922467, 4.897644413504528060, -222.5335369890782999 ) ) ;
#20648 = CARTESIAN_POINT ( 'NONE',  ( 14.82579616070250417, 22.96152595385638762, -233.8920860146931489 ) ) ;
#20649 = CARTESIAN_POINT ( 'NONE',  ( 14.68951511424354273, -18.85605729411972575, -217.5026406474102885 ) ) ;
#20650 = FACE_OUTER_BOUND ( 'NONE', #9647, .T. ) ;
#20651 = ORIENTED_EDGE ( 'NONE', *, *, #6499, .T. ) ;
#20652 = CARTESIAN_POINT ( 'NONE',  ( 1.217121169770782663, 15.31158828575123110, -230.6845728599757308 ) ) ;
#20653 = CARTESIAN_POINT ( 'NONE',  ( -10.04615645102154886, -9.695712423306433791, -230.4834384258168996 ) ) ;
#20654 = DIRECTION ( 'NONE',  ( 0.000000000000000000, 0.000000000000000000, -1.000000000000000000 ) ) ;
#20655 = CARTESIAN_POINT ( 'NONE',  ( 16.00819137755116373, 4.595691552992191120, -229.5669508871464757 ) ) ;
#20656 = CARTESIAN_POINT ( 'NONE',  ( -16.63766460830045091, 5.158675778507696208, -232.1659425527909093 ) ) ;
#20657 = CARTESIAN_POINT ( 'NONE',  ( 21.30961698559626427, -20.48616475849644303, -228.5322376518520002 ) ) ;
#20658 = DIRECTION ( 'NONE',  ( 0.000000000000000000, 0.000000000000000000, 1.000000000000000000 ) ) ;
#20659 = CARTESIAN_POINT ( 'NONE',  ( -22.47200958260654957, 4.697452857301940732, -216.5879371680706242 ) ) ;
#20660 = CARTESIAN_POINT ( 'NONE',  ( -29.95012366401462955, 4.746560250930182967, -224.6954343660969471 ) ) ;
#20661 = CARTESIAN_POINT ( 'NONE',  ( -6.776147227169700749, -16.68571135823561846, -231.0772860317820232 ) ) ;
#20662 = DIRECTION ( 'NONE',  ( -1.000000000000000000, -6.982962677686272233E-15, 0.000000000000000000 ) ) ;
#20663 = CARTESIAN_POINT ( 'NONE',  ( -21.31134010702326975, 8.651877420333450530, 5.025164282198873344 ) ) ;
#20664 = CARTESIAN_POINT ( 'NONE',  ( -25.80904414196669450, 12.19501778665756220, -219.1732313092283846 ) ) ;
#20665 = CARTESIAN_POINT ( 'NONE',  ( 10.87273020620571629, -12.78363999705779186, -228.8712466752294858 ) ) ;
#20666 = CARTESIAN_POINT ( 'NONE',  ( 12.85121247375660047, -2.863977387274604602, -224.0868061481347127 ) ) ;
#20667 = CARTESIAN_POINT ( 'NONE',  ( -23.45512409874873683, 8.653582270224204009, 5.022182943822000922 ) ) ;
#20668 = CARTESIAN_POINT ( 'NONE',  ( 5.909674498212842408, 15.76475534640655773, -228.4922217450045139 ) ) ;
#20669 = CARTESIAN_POINT ( 'NONE',  ( -13.58389614404818069, 15.11490620317918676, -215.3922994348461941 ) ) ;
#20670 = CARTESIAN_POINT ( 'NONE',  ( 12.94599882983645145, 15.82237817288049442, -219.3332542656393116 ) ) ;
#20671 = CARTESIAN_POINT ( 'NONE',  ( -4.572289063834428013, -16.67516242687949557, -229.9678395161569142 ) ) ;
#20672 = VECTOR ( 'NONE', #1693, 1000.000000000000000 ) ;
#20673 = CARTESIAN_POINT ( 'NONE',  ( 30.13983206778957324, -7.413543662652124944, -226.8644184361555745 ) ) ;
#20674 = VERTEX_POINT ( 'NONE', #9178 ) ;
#20675 = CIRCLE ( 'NONE', #10985, 10.76794919243112325 ) ;
#20676 = CARTESIAN_POINT ( 'NONE',  ( -17.99720854823001659, 13.97888873227035056, -232.2992184661552244 ) ) ;
#20677 = CARTESIAN_POINT ( 'NONE',  ( -26.04932551096112192, 5.001193774903864409, -228.9498367494266802 ) ) ;
#20678 = CARTESIAN_POINT ( 'NONE',  ( -11.36937006530106586, 5.486019310970209339, -224.0742584078730033 ) ) ;
#20679 = CARTESIAN_POINT ( 'NONE',  ( -3.968800477764047319, -14.91200208314756104, -226.8245746385127575 ) ) ;
#20680 = CARTESIAN_POINT ( 'NONE',  ( -22.96914677622851642, 2.813105434284154191E-15, 75.00000000000000000 ) ) ;
#20681 = ORIENTED_EDGE ( 'NONE', *, *, #8464, .F. ) ;
#20682 = CARTESIAN_POINT ( 'NONE',  ( 19.66580438618080251, 15.18147523775131624, -233.5153994334876586 ) ) ;
#20683 = CARTESIAN_POINT ( 'NONE',  ( 7.956221944547102964, -16.14435353399512252, -220.6073666753051441 ) ) ;
#20684 = CARTESIAN_POINT ( 'NONE',  ( 7.639528166734322667, 11.92751229241157596, -224.6077814063189635 ) ) ;
#20685 = CARTESIAN_POINT ( 'NONE',  ( -9.443239614166923701, 9.388015667058336788, -222.3195230688234290 ) ) ;
#20686 = EDGE_CURVE ( 'NONE', #237, #6741, #13400, .T. ) ;
#20687 = CIRCLE ( 'NONE', #11006, 21.63401512838748175 ) ;
#20688 = CARTESIAN_POINT ( 'NONE',  ( 19.49137065790598555, 9.165486118354671419, -234.8706749352814995 ) ) ;
#20689 = AXIS2_PLACEMENT_3D ( 'NONE', #3510, #10390, #10610 ) ;
#20690 = EDGE_CURVE ( 'NONE', #18856, #16533, #22021, .T. ) ;
#20691 = CARTESIAN_POINT ( 'NONE',  ( 9.333020543840051531, 16.91085096921651143, -217.7308990335875762 ) ) ;
#20692 = CARTESIAN_POINT ( 'NONE',  ( 1.665334536937734811E-13, -24.63401512838747820, -77.51594804401857175 ) ) ;
#20693 = ADVANCED_FACE ( 'NONE', ( #16250 ), #10900, .T. ) ;
#20694 = CARTESIAN_POINT ( 'NONE',  ( -1.308474130992312023, -24.58654860180777391, -216.2430112183533026 ) ) ;
#20695 = CARTESIAN_POINT ( 'NONE',  ( 19.06212547406409641, -9.287000003594721775, -232.7453815625877667 ) ) ;
#20696 = CARTESIAN_POINT ( 'NONE',  ( 0.000000000000000000, -23.00000000000000000, -60.00000000000000000 ) ) ;
#20697 = CARTESIAN_POINT ( 'NONE',  ( 1.322875655532295358, 1.500000000000000000, -104.9999999999999858 ) ) ;
#20698 = CARTESIAN_POINT ( 'NONE',  ( 25.69300549816939494, 5.947472783069708946, -230.6131061331718115 ) ) ;
#20699 = CARTESIAN_POINT ( 'NONE',  ( -14.94274040728286046, -6.247332224397157852, -226.1562440284360491 ) ) ;
#20700 = CARTESIAN_POINT ( 'NONE',  ( -22.10934047915427314, 0.9940043559354312386, -216.9999999999999716 ) ) ;
#20701 = CARTESIAN_POINT ( 'NONE',  ( 2.471164685565028662, 14.01327037412690935, -223.4905256513065410 ) ) ;
#20702 = CARTESIAN_POINT ( 'NONE',  ( 0.07890756785233743464, 25.14108539708653822, -218.4152285319504756 ) ) ;
#20703 = EDGE_LOOP ( 'NONE', ( #5039, #2135, #20811, #15412 ) ) ;
#20704 = CARTESIAN_POINT ( 'NONE',  ( 25.75143957690053753, -9.476334075918805055, -216.1442976756887617 ) ) ;
#20705 = AXIS2_PLACEMENT_3D ( 'NONE', #4838, #11714, #10556 ) ;
#20706 = CARTESIAN_POINT ( 'NONE',  ( 18.29617186523616468, 23.20920553663278341, -223.4372550713720216 ) ) ;
#20707 = CARTESIAN_POINT ( 'NONE',  ( -15.46752262371512820, 15.15798787883389487, -233.5981584775992701 ) ) ;
#20708 = CARTESIAN_POINT ( 'NONE',  ( -26.88784739727922357, 10.07520213145270915, -227.1866063047054922 ) ) ;
#20709 = CARTESIAN_POINT ( 'NONE',  ( -8.465333986790207987, -12.59497810381903982, -228.1424919783533198 ) ) ;
#20710 = DIRECTION ( 'NONE',  ( 1.000000000000000000, 0.000000000000000000, 0.000000000000000000 ) ) ;
#20711 = CARTESIAN_POINT ( 'NONE',  ( 24.81079154715000357, 3.171651085595392772, -216.4177249688571578 ) ) ;
#20712 = CARTESIAN_POINT ( 'NONE',  ( -8.985448925281199095, 11.82743561134668475, -224.1067108988273162 ) ) ;
#20713 = CARTESIAN_POINT ( 'NONE',  ( 15.89102655998366664, 24.10108298038447572, -232.7733025413564008 ) ) ;
#20714 = CARTESIAN_POINT ( 'NONE',  ( 25.40954707198727647, 2.077273811637330159, -219.3610170479527426 ) ) ;
#20715 = CARTESIAN_POINT ( 'NONE',  ( -32.05942529185317369, -1.254016050025921425, -226.3193970476597485 ) ) ;
#20716 = CARTESIAN_POINT ( 'NONE',  ( -13.08346052978740914, -7.620079078745922274, -220.3923444982454498 ) ) ;
#20717 = CARTESIAN_POINT ( 'NONE',  ( -9.491065840222427497, 13.31995980477872266, -232.8537120564120073 ) ) ;
#20718 = CARTESIAN_POINT ( 'NONE',  ( 1.127544764349826867, -27.89617517048659323, -231.9509945439240823 ) ) ;
#20719 = CARTESIAN_POINT ( 'NONE',  ( -3.673551555920188783, 29.81207051619892923, -228.8770490300152005 ) ) ;
#20720 = CARTESIAN_POINT ( 'NONE',  ( 19.73224149047082321, -2.635265996080750295, -233.5133592171236501 ) ) ;
#20721 = CARTESIAN_POINT ( 'NONE',  ( -29.27492217116574480, -1.185422171198730501, -224.8132346143397342 ) ) ;
#20722 = CARTESIAN_POINT ( 'NONE',  ( -18.05576253097465766, 2.935622250037499104, -232.1557308718028594 ) ) ;
#20723 = CARTESIAN_POINT ( 'NONE',  ( 0.000000000000000000, 0.000000000000000000, 75.00000000000000000 ) ) ;
#20724 = ADVANCED_FACE ( 'NONE', ( #10852 ), #12331, .F. ) ;
#20725 = CARTESIAN_POINT ( 'NONE',  ( -0.2748333203896175525, 17.57683079704640505, -221.1444293135629948 ) ) ;
#20726 = CARTESIAN_POINT ( 'NONE',  ( 15.14536540539411114, 2.907144070186200580, -217.8738854795238922 ) ) ;
#20727 = CARTESIAN_POINT ( 'NONE',  ( 19.72515656911863147, 14.02277373989196541, -218.0718040828188009 ) ) ;
#20728 = CARTESIAN_POINT ( 'NONE',  ( 26.72610819325501907, 14.97064052581051108, -224.6384473985499426 ) ) ;
#20729 = CARTESIAN_POINT ( 'NONE',  ( -1.925327751674894339, -31.30071588347811584, -225.0681195224254623 ) ) ;
#20730 = CARTESIAN_POINT ( 'NONE',  ( 3.711349367426693746, 16.84755988915346236, -233.7359972593521888 ) ) ;
#20731 = DIRECTION ( 'NONE',  ( 0.000000000000000000, 0.000000000000000000, -1.000000000000000000 ) ) ;
#20732 = CARTESIAN_POINT ( 'NONE',  ( -12.81114484120449504, -26.81657559919244349, -231.7433950434849805 ) ) ;
#20733 = CARTESIAN_POINT ( 'NONE',  ( -10.70754874174748039, 23.84972878377777405, -230.7991598016655246 ) ) ;
#20734 = CARTESIAN_POINT ( 'NONE',  ( 17.24952650401854370, 25.19767938110938843, -224.5319471861414797 ) ) ;
#20735 = CARTESIAN_POINT ( 'NONE',  ( -18.34948365288241590, -1.907751280579004893, -231.5848060246952116 ) ) ;
#20736 = CARTESIAN_POINT ( 'NONE',  ( -14.01525440049806193, 8.239250543314939890, -226.5804714421811070 ) ) ;
#20737 = CARTESIAN_POINT ( 'NONE',  ( -22.70558257617108922, 14.65737936663030538, -230.9775454010380997 ) ) ;
#20738 = CARTESIAN_POINT ( 'NONE',  ( 21.14328650935969023, 6.072767611243683916, -217.6422864096696514 ) ) ;
#20739 = ORIENTED_EDGE ( 'NONE', *, *, #16711, .T. ) ;
#20740 = CARTESIAN_POINT ( 'NONE',  ( 17.60676319847677007, 21.31475060840986302, -219.8266339603936785 ) ) ;
#20741 = CARTESIAN_POINT ( 'NONE',  ( 13.35408364068459619, -22.25650632745845314, -229.3239852056058226 ) ) ;
#20742 = ORIENTED_EDGE ( 'NONE', *, *, #12429, .T. ) ;
#20743 = CARTESIAN_POINT ( 'NONE',  ( 24.05238142633148968, -17.07083877791421500, -221.4615098029387070 ) ) ;
#20744 = CARTESIAN_POINT ( 'NONE',  ( 1.030230143518703345, 18.27887886751213387, -229.5791973322770616 ) ) ;
#20745 = CARTESIAN_POINT ( 'NONE',  ( 0.000000000000000000, 19.63401512838747820, -77.51594804401857175 ) ) ;
#20746 = CARTESIAN_POINT ( 'NONE',  ( 14.68783945462866924, 9.535285537539673228, -219.4694094309942045 ) ) ;
#20747 = CARTESIAN_POINT ( 'NONE',  ( -23.03165807712271373, -11.67016847039487892, -215.7330867557714384 ) ) ;
#20748 = CARTESIAN_POINT ( 'NONE',  ( -5.420780812268581883, -12.08122409751860360, -226.5143039284326392 ) ) ;
#20749 = CARTESIAN_POINT ( 'NONE',  ( 1.752757082432757185, -17.15725705531007250, -232.7539178101738742 ) ) ;
#20750 = CARTESIAN_POINT ( 'NONE',  ( -2.693916085894628942, 18.86613858709357672, -230.4911878356387263 ) ) ;
#20751 = DIRECTION ( 'NONE',  ( 0.000000000000000000, 0.000000000000000000, -1.000000000000000000 ) ) ;
#20752 = CARTESIAN_POINT ( 'NONE',  ( 27.66944030902029539, 6.857614156517904291, -220.9860880211026313 ) ) ;
#20753 = CARTESIAN_POINT ( 'NONE',  ( -20.54164754914381064, 7.122791156791981493, -233.5720402887671980 ) ) ;
#20754 = CARTESIAN_POINT ( 'NONE',  ( -8.316066124693966444, 26.67103469786491843, -222.2304303634109885 ) ) ;
#20755 = CARTESIAN_POINT ( 'NONE',  ( 3.367418898937407867, 27.20023797116225595, -219.3349021808245709 ) ) ;
#20756 = CARTESIAN_POINT ( 'NONE',  ( 12.93042813863272755, 0.4488092930645843914, -225.5263188864764174 ) ) ;
#20757 = CARTESIAN_POINT ( 'NONE',  ( 17.65694480011521250, 15.62497337860048674, -235.2008064134603273 ) ) ;
#20758 = CARTESIAN_POINT ( 'NONE',  ( 9.338484253624125486, -13.53666216847648052, -219.8958652322373837 ) ) ;
#20759 = DIRECTION ( 'NONE',  ( -0.000000000000000000, -0.000000000000000000, 1.000000000000000000 ) ) ;
#20760 = EDGE_LOOP ( 'NONE', ( #2243, #4011, #5067, #12363 ) ) ;
#20761 = CARTESIAN_POINT ( 'NONE',  ( -2.772442535524381579, 13.75675912271027457, -228.9770533867650215 ) ) ;
#20762 = CARTESIAN_POINT ( 'NONE',  ( -22.35595593184171292, -2.191382721379458332, -235.3044553127160441 ) ) ;
#20763 = CARTESIAN_POINT ( 'NONE',  ( 23.48720700658024896, -2.145453947144424500, -217.8824464111000054 ) ) ;
#20764 = CARTESIAN_POINT ( 'NONE',  ( 13.43730899468209294, 8.427513769504761498, -221.4030804848920297 ) ) ;
#20765 = CARTESIAN_POINT ( 'NONE',  ( -20.94800339253696109, 4.477632454355491731, -216.5423208360950298 ) ) ;
#20766 = CARTESIAN_POINT ( 'NONE',  ( 8.532614294830283441, -28.73326933124977955, -229.1610356131385231 ) ) ;
#20767 = DIRECTION ( 'NONE',  ( 0.000000000000000000, 0.000000000000000000, 1.000000000000000000 ) ) ;
#20768 = CARTESIAN_POINT ( 'NONE',  ( -7.189383125363055349, 14.28512618638020548, -231.7475838278701303 ) ) ;
#20769 = CARTESIAN_POINT ( 'NONE',  ( -21.89065952084848021, -0.9940043559354364566, -216.9999999999999716 ) ) ;
#20770 = CARTESIAN_POINT ( 'NONE',  ( -5.805911442544755552, -26.83424102279996504, -229.6222293353685302 ) ) ;
#20771 = DIRECTION ( 'NONE',  ( 1.000000000000000000, 6.982962677686272233E-15, 0.000000000000000000 ) ) ;
#20772 = DIRECTION ( 'NONE',  ( -1.000000000000000000, 0.000000000000000000, 0.000000000000000000 ) ) ;
#20773 = CARTESIAN_POINT ( 'NONE',  ( -13.10651848559790444, 3.262242204071156948, -224.3513854875720597 ) ) ;
#20774 = CARTESIAN_POINT ( 'NONE',  ( 23.15933523859005660, -14.47549635653155775, -222.2572217030593436 ) ) ;
#20775 = CARTESIAN_POINT ( 'NONE',  ( -24.25245498015852874, 0.2109992039763788352, -218.1398602137601301 ) ) ;
#20776 = CARTESIAN_POINT ( 'NONE',  ( 18.92955364685788666, -2.856280672885344263, -225.9473756571962042 ) ) ;
#20777 = CARTESIAN_POINT ( 'NONE',  ( 12.98277799799954124, 10.30128574332056779, -221.9415428419440559 ) ) ;
#20778 = CARTESIAN_POINT ( 'NONE',  ( -7.686214453470440411, 10.71593237010305444, -228.8058998235944159 ) ) ;
#20779 = CIRCLE ( 'NONE', #21498, 12.50000000000000000 ) ;
#20780 = CARTESIAN_POINT ( 'NONE',  ( 13.17424634425744046, 10.51488364724239588, -221.4616598107521099 ) ) ;
#20781 = CARTESIAN_POINT ( 'NONE',  ( 0.7148793108008648645, -17.78534256477599840, -218.6573294195452775 ) ) ;
#20782 = CARTESIAN_POINT ( 'NONE',  ( 27.83450977899788370, 1.364662819714677511, -230.5442677252456463 ) ) ;
#20783 = VERTEX_POINT ( 'NONE', #613 ) ;
#20784 = CARTESIAN_POINT ( 'NONE',  ( -4.386767007475907754, 14.39570986262862107, -223.2690175027443615 ) ) ;
#20785 = CARTESIAN_POINT ( 'NONE',  ( -14.59766675578715223, 7.926254675926275972, -222.3706877972550444 ) ) ;
#20786 = CARTESIAN_POINT ( 'NONE',  ( -12.13127060986278316, 5.971392262169284315, -229.0615017441034524 ) ) ;
#20787 = ORIENTED_EDGE ( 'NONE', *, *, #8177, .T. ) ;
#20788 = CARTESIAN_POINT ( 'NONE',  ( -11.98034293927688765, -10.98662817740026121, -223.7553339400932373 ) ) ;
#20789 = CARTESIAN_POINT ( 'NONE',  ( 0.000000000000000000, 0.000000000000000000, -30.00000000000000000 ) ) ;
#20790 = ORIENTED_EDGE ( 'NONE', *, *, #18966, .F. ) ;
#20791 = CARTESIAN_POINT ( 'NONE',  ( 16.20788843645364352, 6.828976201867700269, -231.6689701909764665 ) ) ;
#20792 = CARTESIAN_POINT ( 'NONE',  ( 12.14783608763084644, -10.95966212275308571, -222.8518398773795184 ) ) ;
#20793 = CARTESIAN_POINT ( 'NONE',  ( 14.68783945462866924, 9.535285537539673228, -219.4694094309942045 ) ) ;
#20794 = CARTESIAN_POINT ( 'NONE',  ( -14.73016414256368911, 22.23431809695627237, -217.1425123644553707 ) ) ;
#20795 =( BOUNDED_CURVE ( )  B_SPLINE_CURVE ( 3, ( #21938, #6529, #13399, #17426 ),
 .UNSPECIFIED., .F., .F. ) 
 B_SPLINE_CURVE_WITH_KNOTS ( ( 4, 4 ),
 ( 3.141592653589793116, 6.283185307179586232 ),
 .UNSPECIFIED. ) 
 CURVE ( )  GEOMETRIC_REPRESENTATION_ITEM ( )  RATIONAL_B_SPLINE_CURVE ( ( 1.000000000000000000, 0.3333333333333333703, 0.3333333333333333703, 1.000000000000000000 ) ) 
 REPRESENTATION_ITEM ( '' )  );
#20796 = AXIS2_PLACEMENT_3D ( 'NONE', #14289, #21122, #650 ) ;
#20797 = CARTESIAN_POINT ( 'NONE',  ( 12.08790845148079640, 6.355304031620478078, -220.0087475230167229 ) ) ;
#20798 = EDGE_CURVE ( 'NONE', #6969, #19507, #16650, .T. ) ;
#20799 = CARTESIAN_POINT ( 'NONE',  ( 1.773982976645536835, 19.12448993322812285, -233.2315972735944172 ) ) ;
#20800 = LINE ( 'NONE', #21024, #20236 ) ;
#20801 = CARTESIAN_POINT ( 'NONE',  ( 8.021672912688133650, -23.92397517040199872, -233.3380040120402441 ) ) ;
#20802 = CARTESIAN_POINT ( 'NONE',  ( 11.39114332821395692, -8.257479203742953189, -226.5648397932267528 ) ) ;
#20803 = DIRECTION ( 'NONE',  ( -0.000000000000000000, 0.000000000000000000, -1.000000000000000000 ) ) ;
#20804 = FACE_OUTER_BOUND ( 'NONE', #21229, .T. ) ;
#20805 = CARTESIAN_POINT ( 'NONE',  ( -23.70973587455150522, 20.45398817402440983, -228.9005348699235469 ) ) ;
#20806 = CARTESIAN_POINT ( 'NONE',  ( -26.46950597041758968, -8.633348373924491170, -225.4226425040951085 ) ) ;
#20807 = EDGE_CURVE ( 'NONE', #18785, #7031, #15928, .T. ) ;
#20808 = CARTESIAN_POINT ( 'NONE',  ( -15.83178333309709629, 2.467763724635483324, -230.4064772870105458 ) ) ;
#20809 = CARTESIAN_POINT ( 'NONE',  ( 8.175342817246784577, 19.41817470142738244, -216.6818271833384699 ) ) ;
#20810 = CARTESIAN_POINT ( 'NONE',  ( -1.973648319964989462, 15.33498294326524203, -220.9958390492969329 ) ) ;
#20811 = ORIENTED_EDGE ( 'NONE', *, *, #13875, .T. ) ;
#20812 = CARTESIAN_POINT ( 'NONE',  ( 12.82249318900957391, -5.922664226158099510, -218.4318038749311768 ) ) ;
#20813 = CARTESIAN_POINT ( 'NONE',  ( 25.69300549816939494, 5.947472783069708946, -230.6131061331718115 ) ) ;
#20814 = CARTESIAN_POINT ( 'NONE',  ( -11.59479561055411345, 9.544396733298208702, -229.1494558965577255 ) ) ;
#20815 = CARTESIAN_POINT ( 'NONE',  ( -27.11599398522282911, 10.60460483532474996, -224.7310548435675912 ) ) ;
#20816 = CARTESIAN_POINT ( 'NONE',  ( -8.978805095734141872, -14.89723076936793156, -219.0730636071341451 ) ) ;
#20817 = CARTESIAN_POINT ( 'NONE',  ( -16.15126510923403202, -0.4755054218165427615, -219.3066569788202571 ) ) ;
#20818 = LINE ( 'NONE', #245, #10498 ) ;
#20819 = CYLINDRICAL_SURFACE ( 'NONE', #16299, 17.50000000000007816 ) ;
#20820 = CARTESIAN_POINT ( 'NONE',  ( -13.12488928717151637, 0.000000000000000000, -99.99999999999998579 ) ) ;
#20821 = CARTESIAN_POINT ( 'NONE',  ( -11.13829636790841704, 14.30978168460582189, -218.6922574227322400 ) ) ;
#20822 = CARTESIAN_POINT ( 'NONE',  ( 10.93653298376230687, 10.42959444671468106, -232.5920418140667039 ) ) ;
#20823 = CARTESIAN_POINT ( 'NONE',  ( -18.46722752239034193, 0.9784074152395518809, -232.1633353206286188 ) ) ;
#20824 = CARTESIAN_POINT ( 'NONE',  ( -32.13037437807204810, -1.025156162654832670, -224.7589498746283141 ) ) ;
#20825 = CARTESIAN_POINT ( 'NONE',  ( -23.85568197540453994, -15.41036827548725618, -219.8503866864575969 ) ) ;
#20826 = CARTESIAN_POINT ( 'NONE',  ( -14.84124724799726991, 21.42277200659090042, -233.6300684249849553 ) ) ;
#20827 = CARTESIAN_POINT ( 'NONE',  ( -8.376153411442972541, -27.59911039556260448, -219.0729038785590888 ) ) ;
#20828 = CARTESIAN_POINT ( 'NONE',  ( 8.812073984913094904, 13.12649198322903210, -229.9172071780580495 ) ) ;
#20829 = CARTESIAN_POINT ( 'NONE',  ( 4.579865149819754677, -13.09122092233156387, -219.1296897471712839 ) ) ;
#20830 = CARTESIAN_POINT ( 'NONE',  ( 0.000000000000000000, -23.00000000000000000, -69.99999999999998579 ) ) ;
#20831 = CARTESIAN_POINT ( 'NONE',  ( -27.92885697401080591, 6.962042978589167319, -220.9552227796709190 ) ) ;
#20832 = PRESENTATION_STYLE_ASSIGNMENT (( #21270 ) ) ;
#20833 = CARTESIAN_POINT ( 'NONE',  ( -5.589224416770360193, 14.13652937339764115, -225.1481999119820330 ) ) ;
#20834 = CARTESIAN_POINT ( 'NONE',  ( -20.00523085820573499, 3.356386534894876927, -232.9491364426554298 ) ) ;
#20835 = CARTESIAN_POINT ( 'NONE',  ( 24.58316096239279602, 5.861425670879941485, -231.3104446318280623 ) ) ;
#20836 = CARTESIAN_POINT ( 'NONE',  ( 15.14859676485869500, 2.119979922547468032, -231.9009926880791284 ) ) ;
#20837 = CARTESIAN_POINT ( 'NONE',  ( 1.444415905432371749, -18.02453083990606331, -216.1804672466811894 ) ) ;
#20838 = CARTESIAN_POINT ( 'NONE',  ( 5.784594921161807513, 11.98867617302893329, -219.3746160931291058 ) ) ;
#20839 = CARTESIAN_POINT ( 'NONE',  ( 27.40550551777678123, 5.967061366481472895, -228.7463788799179554 ) ) ;
#20840 = CARTESIAN_POINT ( 'NONE',  ( -5.131528111146875126, -19.01772154664624992, -215.2265844479019563 ) ) ;
#20841 = CARTESIAN_POINT ( 'NONE',  ( -4.142636420702924482, 14.17169704882741321, -225.1666440184957310 ) ) ;
#20842 = CARTESIAN_POINT ( 'NONE',  ( 7.213476267053916757, 16.78447451494783138, -217.5857052077849687 ) ) ;
#20843 = CARTESIAN_POINT ( 'NONE',  ( -18.11268275035277853, -3.459088653808292335, -218.4233329573673359 ) ) ;
#20844 = CARTESIAN_POINT ( 'NONE',  ( -18.33565906012873725, 9.491905303418088025, -219.1855745749628568 ) ) ;
#20845 = CLOSED_SHELL ( 'NONE', ( #9418, #18753, #18920, #20506, #17920, #8663, #2572, #3447, #186, #8611, #18400, #11272, #11071, #13538, #9907, #18871, #5396, #10381, #4521, #12840, #8578, #7367, #15757 ) ) ;
#20846 = CARTESIAN_POINT ( 'NONE',  ( -5.028549462823471039, 18.55099042571767143, -234.6264744246184648 ) ) ;
#20847 = CARTESIAN_POINT ( 'NONE',  ( 16.77055746703809191, 7.081497542956901370, -232.0295235404293521 ) ) ;
#20848 = ORIENTED_EDGE ( 'NONE', *, *, #19998, .F. ) ;
#20849 = CARTESIAN_POINT ( 'NONE',  ( 7.033108278341462238, -17.71891568601925826, -230.1509483552532060 ) ) ;
#20850 = ORIENTED_EDGE ( 'NONE', *, *, #6311, .F. ) ;
#20851 = CARTESIAN_POINT ( 'NONE',  ( 8.211296573249146746, -12.45047565346596130, -222.1279395315445413 ) ) ;
#20852 = CARTESIAN_POINT ( 'NONE',  ( -6.067446494494625142, 16.28408815813367028, -230.0786439517394513 ) ) ;
#20853 = VERTEX_POINT ( 'NONE', #19615 ) ;
#20854 = CARTESIAN_POINT ( 'NONE',  ( 12.99034161053428349, 11.71468708507361889, -230.9043293568357740 ) ) ;
#20855 = CARTESIAN_POINT ( 'NONE',  ( 22.36788034568564854, -2.140002702436959225, -217.7104380410378610 ) ) ;
#20856 = CARTESIAN_POINT ( 'NONE',  ( -25.10035252441274167, -15.33546242866430198, -228.3913311683031964 ) ) ;
#20857 = CARTESIAN_POINT ( 'NONE',  ( 3.342529885312644833, -17.78621320651278737, -216.7788622297345853 ) ) ;
#20858 = CARTESIAN_POINT ( 'NONE',  ( -5.589224416770360193, 14.13652937339764115, -225.1481999119820330 ) ) ;
#20859 = DIRECTION ( 'NONE',  ( 1.000000000000000000, 0.000000000000000000, 0.000000000000000000 ) ) ;
#20860 = CARTESIAN_POINT ( 'NONE',  ( 24.93482953594869755, 13.13888391581411241, -222.4369546851285691 ) ) ;
#20861 = EDGE_CURVE ( 'NONE', #566, #6655, #11079, .T. ) ;
#20862 = CARTESIAN_POINT ( 'NONE',  ( -11.02345917017863464, 29.02019856777526741, -223.9475008740665771 ) ) ;
#20863 = CARTESIAN_POINT ( 'NONE',  ( -8.137644474477026435, 12.10064032984799098, -226.6735072060122036 ) ) ;
#20864 = CARTESIAN_POINT ( 'NONE',  ( 10.40160332990717151, 27.59713857063802323, -221.5374724512453213 ) ) ;
#20865 = CARTESIAN_POINT ( 'NONE',  ( -16.88145396433676027, 5.002512658926777434, -221.2364783498041731 ) ) ;
#20866 = CARTESIAN_POINT ( 'NONE',  ( 16.53896178738450828, 2.691624496798088462, -232.5974196329879078 ) ) ;
#20867 = CARTESIAN_POINT ( 'NONE',  ( 18.24334571313621467, -21.83696521683136282, -220.5798317591433886 ) ) ;
#20868 = FACE_OUTER_BOUND ( 'NONE', #5101, .T. ) ;
#20869 = ORIENTED_EDGE ( 'NONE', *, *, #13238, .T. ) ;
#20870 = CARTESIAN_POINT ( 'NONE',  ( -2.934221234790329369, 15.07857928364152222, -230.9558365497803720 ) ) ;
#20871 = CARTESIAN_POINT ( 'NONE',  ( 22.26090851979669338, -3.689523054771738586, -218.9825289563843285 ) ) ;
#20872 = DIRECTION ( 'NONE',  ( 0.000000000000000000, 0.000000000000000000, -1.000000000000000000 ) ) ;
#20873 = CARTESIAN_POINT ( 'NONE',  ( 24.42567939027770407, 10.22651298688739097, -219.4562066833365748 ) ) ;
#20874 = CARTESIAN_POINT ( 'NONE',  ( -24.48580119005125866, 9.312492396273500006, -232.5498413856076070 ) ) ;
#20875 = CARTESIAN_POINT ( 'NONE',  ( 5.668262076144046979, -25.28042871382391965, -216.8182873783340483 ) ) ;
#20876 = CARTESIAN_POINT ( 'NONE',  ( 0.000000000000000000, 0.000000000000000000, 0.000000000000000000 ) ) ;
#20877 = CARTESIAN_POINT ( 'NONE',  ( -24.02434186778878455, 18.57431834865475651, -228.2662945587547370 ) ) ;
#20878 = CARTESIAN_POINT ( 'NONE',  ( -16.09559989144903369, 12.31939076846282966, -216.7948290530243298 ) ) ;
#20879 = VERTEX_POINT ( 'NONE', #17508 ) ;
#20880 = CARTESIAN_POINT ( 'NONE',  ( -28.99926036811508467, 3.909990568804979194, -228.9613767892386988 ) ) ;
#20881 = CARTESIAN_POINT ( 'NONE',  ( -15.43902962033193837, -12.71219713885795422, -232.7078469548986845 ) ) ;
#20882 = CARTESIAN_POINT ( 'NONE',  ( 0.000000000000000000, 17.50000000000000711, -30.00000000000000000 ) ) ;
#20883 = CARTESIAN_POINT ( 'NONE',  ( 15.52031161554735128, 1.026483668354684076, -227.8437971491433132 ) ) ;
#20884 = CARTESIAN_POINT ( 'NONE',  ( -11.67631226053870996, 6.737291529340801333, -227.3110382950315227 ) ) ;
#20885 = CARTESIAN_POINT ( 'NONE',  ( 7.357019007885960526, -24.37006613449481662, -217.4041786725384782 ) ) ;
#20886 = CARTESIAN_POINT ( 'NONE',  ( 2.465190328815661892E-29, 25.00000000000012790, -75.00000000000000000 ) ) ;
#20887 = EDGE_CURVE ( 'NONE', #21087, #13000, #8475, .T. ) ;
#20888 = CARTESIAN_POINT ( 'NONE',  ( 21.68053922431529301, 13.05890675940072931, -230.5667798303363440 ) ) ;
#20889 = CARTESIAN_POINT ( 'NONE',  ( -18.07648963816576781, 14.36622924931724654, -235.1425738388569187 ) ) ;
#20890 = CARTESIAN_POINT ( 'NONE',  ( -2.000000000000000000, 2.449293598294706414E-16, -120.0000000000000142 ) ) ;
#20891 = CARTESIAN_POINT ( 'NONE',  ( 15.20072702475037296, 19.31591084219522614, -219.7402199933931399 ) ) ;
#20892 = CARTESIAN_POINT ( 'NONE',  ( -3.614824051224299950, -15.07124992037100064, -223.1721701483932065 ) ) ;
#20893 = CARTESIAN_POINT ( 'NONE',  ( 25.70000612522241568, -7.596455516557234944, -216.8500112287931074 ) ) ;
#20894 = ORIENTED_EDGE ( 'NONE', *, *, #17864, .T. ) ;
#20895 = CARTESIAN_POINT ( 'NONE',  ( -4.879985665934096772, 15.33285679834440174, -220.9402849574511833 ) ) ;
#20896 = CARTESIAN_POINT ( 'NONE',  ( -26.64664107080812627, 5.256684826493772000, -228.0533579629717735 ) ) ;
#20897 = CARTESIAN_POINT ( 'NONE',  ( -26.47501633019681577, 13.84484755257420119, -230.0154374881822719 ) ) ;
#20898 = AXIS2_PLACEMENT_3D ( 'NONE', #2143, #12397, #8913 ) ;
#20899 = ORIENTED_EDGE ( 'NONE', *, *, #18433, .T. ) ;
#20900 = CARTESIAN_POINT ( 'NONE',  ( -11.82770121052164924, -14.33821066513346487, -229.8071374592849452 ) ) ;
#20901 = VERTEX_POINT ( 'NONE', #17838 ) ;
#20902 = CARTESIAN_POINT ( 'NONE',  ( 25.40954707198727647, 2.077273811637330159, -219.3610170479527426 ) ) ;
#20903 = CARTESIAN_POINT ( 'NONE',  ( 3.242550426224029447, -16.70085388461110654, -229.1030317736733650 ) ) ;
#20904 = CARTESIAN_POINT ( 'NONE',  ( 22.46220731426537043, 18.23201731183003460, -227.5436199598787539 ) ) ;
#20905 = CARTESIAN_POINT ( 'NONE',  ( -7.395406416482832590, 12.93623984139929739, -219.2606224730616873 ) ) ;
#20906 = CIRCLE ( 'NONE', #17676, 21.50000000000001066 ) ;
#20907 = ADVANCED_BREP_SHAPE_REPRESENTATION ( '', ( #21952, #6677 ), #13476 ) ;
#20908 = CARTESIAN_POINT ( 'NONE',  ( 20.82555317450757215, 14.06078233701296476, -215.4201375757437802 ) ) ;
#20909 = AXIS2_PLACEMENT_3D ( 'NONE', #11250, #2575, #14744 ) ;
#20910 = CARTESIAN_POINT ( 'NONE',  ( 4.656903975822286768, 13.45000048768594780, -227.6722060245555497 ) ) ;
#20911 = CARTESIAN_POINT ( 'NONE',  ( 14.44151618910354706, 2.059759062152056064, -222.8188548941175782 ) ) ;
#20912 = CARTESIAN_POINT ( 'NONE',  ( -7.832594822155400927, -23.57318293858060088, -216.4298491688572028 ) ) ;
#20913 = CARTESIAN_POINT ( 'NONE',  ( 21.39922646226391478, -21.53954253117021977, -224.1701659532164967 ) ) ;
#20914 = CARTESIAN_POINT ( 'NONE',  ( 0.000000000000000000, 0.000000000000000000, -24.99999999999999645 ) ) ;
#20915 = CARTESIAN_POINT ( 'NONE',  ( 0.000000000000000000, 0.000000000000000000, 77.51594804401857175 ) ) ;
#20916 = CARTESIAN_POINT ( 'NONE',  ( -10.98447002683091256, 8.146786682930290624, -230.8316952156193338 ) ) ;
#20917 = CARTESIAN_POINT ( 'NONE',  ( 25.14972984070899997, 1.185371537549434029, -234.2576837523010909 ) ) ;
#20918 = CARTESIAN_POINT ( 'NONE',  ( 20.47387447818710271, 7.390772095927000684, -234.0991886097562258 ) ) ;
#20919 = CARTESIAN_POINT ( 'NONE',  ( 2.579827969572558111, 15.91317371615649101, -219.7652087782269916 ) ) ;
#20920 = CARTESIAN_POINT ( 'NONE',  ( -0.4548635697939061306, 27.30478022265488036, -219.8474162243132071 ) ) ;
#20921 = ORIENTED_EDGE ( 'NONE', *, *, #6066, .F. ) ;
#20922 = CARTESIAN_POINT ( 'NONE',  ( 20.78003164828882632, -23.67023879211220461, -227.8573985392403074 ) ) ;
#20923 = ORIENTED_EDGE ( 'NONE', *, *, #18546, .F. ) ;
#20924 = CARTESIAN_POINT ( 'NONE',  ( 16.84848658399567611, 11.39632653812981644, -217.9589513831453473 ) ) ;
#20925 = EDGE_CURVE ( 'NONE', #2791, #12254, #3795, .T. ) ;
#20926 = AXIS2_PLACEMENT_3D ( 'NONE', #20915, #17666, #7211 ) ;
#20927 = CARTESIAN_POINT ( 'NONE',  ( -22.57859951143173660, 16.82392524473188899, -219.5628058978911383 ) ) ;
#20928 = CARTESIAN_POINT ( 'NONE',  ( -12.99458409358603284, 11.56864380452031504, -232.0274663316965018 ) ) ;
#20929 = CARTESIAN_POINT ( 'NONE',  ( -26.09107693309126574, -10.38942742183557399, -230.9365759677854442 ) ) ;
#20930 = CARTESIAN_POINT ( 'NONE',  ( -18.39892766464214446, 25.11039525536027739, -225.3444503920457294 ) ) ;
#20931 = DIRECTION ( 'NONE',  ( -1.000000000000000000, 0.000000000000000000, 0.000000000000000000 ) ) ;
#20932 = CARTESIAN_POINT ( 'NONE',  ( 14.83290459615719215, -2.296615622475745688, -226.9301701175285757 ) ) ;
#20933 = CARTESIAN_POINT ( 'NONE',  ( 14.32449519560807438, 0.8432996792098175209, -220.3117614177709527 ) ) ;
#20934 = CARTESIAN_POINT ( 'NONE',  ( -13.14888680331901583, 26.03314517226533908, -227.7900104434697539 ) ) ;
#20935 = CARTESIAN_POINT ( 'NONE',  ( 14.75291830987536557, 13.43762972591284033, -235.1407057970265839 ) ) ;
#20936 = CARTESIAN_POINT ( 'NONE',  ( 21.83031488337932657, -1.542591969257240070, -231.3901500139511427 ) ) ;
#20937 = CIRCLE ( 'NONE', #1898, 22.97235139684061878 ) ;
#20938 = CARTESIAN_POINT ( 'NONE',  ( -11.66037817688884992, -1.871521667041048609, -223.1840616512448037 ) ) ;
#20939 = CARTESIAN_POINT ( 'NONE',  ( -12.18037021406049547, -6.685450889859271051, -226.7642181357440734 ) ) ;
#20940 = CARTESIAN_POINT ( 'NONE',  ( -23.95129667199961077, 20.99391807043993552, -227.1541646794576081 ) ) ;
#20941 = CARTESIAN_POINT ( 'NONE',  ( -2.576162127940193169, -15.57202066281789321, -231.6911579627040396 ) ) ;
#20942 = CARTESIAN_POINT ( 'NONE',  ( 10.07175337281514871, 14.76776740066196325, -231.7834566702614723 ) ) ;
#20943 = CARTESIAN_POINT ( 'NONE',  ( 14.31773767102621875, -28.01644431351170894, -220.7875045263454865 ) ) ;
#20944 = CARTESIAN_POINT ( 'NONE',  ( 14.44752737957290734, -0.3096824834134420112, -227.9839733948226410 ) ) ;
#20945 = CARTESIAN_POINT ( 'NONE',  ( -16.81936022032888545, 5.700806722825413786, -218.5726178058217215 ) ) ;
#20946 = SURFACE_STYLE_FILL_AREA ( #12412 ) ;
#20947 = CARTESIAN_POINT ( 'NONE',  ( -7.058999618647554541, 24.62458660126260312, -219.6630466582859356 ) ) ;
#20948 = CARTESIAN_POINT ( 'NONE',  ( -28.61025869263052712, 6.891613135096296361, -222.2489362813765013 ) ) ;
#20949 = CARTESIAN_POINT ( 'NONE',  ( 23.49048926389013658, 9.645778135078892035, -218.7307869890797463 ) ) ;
#20950 = CARTESIAN_POINT ( 'NONE',  ( 20.88350594575732799, 13.65521425050155813, -232.8060468608549911 ) ) ;
#20951 = CARTESIAN_POINT ( 'NONE',  ( -9.979217823323752512, -26.65442139683551659, -219.8174849573283325 ) ) ;
#20952 = CARTESIAN_POINT ( 'NONE',  ( 18.26039090677515375, 26.14311541888654844, -228.1864986152887127 ) ) ;
#20953 = VECTOR ( 'NONE', #10770, 1000.000000000000000 ) ;
#20954 = DIRECTION ( 'NONE',  ( -1.000000000000000000, 0.000000000000000000, 0.000000000000000000 ) ) ;
#20955 = CARTESIAN_POINT ( 'NONE',  ( -12.24325066776002657, -20.13554689852184509, -214.7483342848939856 ) ) ;
#20956 = CARTESIAN_POINT ( 'NONE',  ( -10.02095171162140019, 11.02119725306997111, -224.1251327387667516 ) ) ;
#20957 = CARTESIAN_POINT ( 'NONE',  ( 8.592982993077152187, 10.20906991731218838, -226.0923132092261483 ) ) ;
#20958 = CARTESIAN_POINT ( 'NONE',  ( -13.91323058514953637, 8.006348396443080162, -225.5064972756604220 ) ) ;
#20959 = ADVANCED_FACE ( 'NONE', ( #2403 ), #7397, .T. ) ;
#20960 = CARTESIAN_POINT ( 'NONE',  ( 1.920320557106582893, 25.99317453242502296, -234.5637964893073217 ) ) ;
#20961 = CARTESIAN_POINT ( 'NONE',  ( 24.60354977307301283, 7.993510024274534942, -218.5358880819990759 ) ) ;
#20962 = EDGE_LOOP ( 'NONE', ( #21999, #12608, #21535, #1068 ) ) ;
#20963 = CARTESIAN_POINT ( 'NONE',  ( 17.63166870185818169, -20.21345786093278107, -221.6360081359454739 ) ) ;
#20964 = ORIENTED_EDGE ( 'NONE', *, *, #2109, .F. ) ;
#20965 = CARTESIAN_POINT ( 'NONE',  ( 12.78854151797817451, -25.92021405714643123, -222.0152117995072842 ) ) ;
#20966 = EDGE_CURVE ( 'NONE', #497, #14323, #6298, .T. ) ;
#20967 = CARTESIAN_POINT ( 'NONE',  ( -8.467651734177735534, 23.23776955534497546, -231.2693664226804913 ) ) ;
#20968 = ORIENTED_EDGE ( 'NONE', *, *, #20477, .T. ) ;
#20969 = CARTESIAN_POINT ( 'NONE',  ( 0.000000000000000000, -25.00000000000000000, 75.00000000000000000 ) ) ;
#20970 = CARTESIAN_POINT ( 'NONE',  ( 9.333020543840051531, 16.91085096921651143, -217.7308990335875762 ) ) ;
#20971 = CARTESIAN_POINT ( 'NONE',  ( 24.21331552874348958, 0.07051084380047288602, -231.7986140076958463 ) ) ;
#20972 = CARTESIAN_POINT ( 'NONE',  ( -21.08965452150356867, -10.66825825602615296, -217.1903588586143314 ) ) ;
#20973 = AXIS2_PLACEMENT_3D ( 'NONE', #11671, #13144, #3108 ) ;
#20974 = CARTESIAN_POINT ( 'NONE',  ( 1.904360901363437275, -12.77109371939166138, -224.5066922355585177 ) ) ;
#20975 = CARTESIAN_POINT ( 'NONE',  ( -0.3589900283600636066, 18.35437183075527656, -220.3960288481451357 ) ) ;
#20976 = LINE ( 'NONE', #19395, #7661 ) ;
#20977 = CARTESIAN_POINT ( 'NONE',  ( 13.80707869872719762, 6.429545566348308760, -225.7152177910682553 ) ) ;
#20978 = CARTESIAN_POINT ( 'NONE',  ( -17.65835845419170624, 22.55329142274348442, -231.2673511165784532 ) ) ;
#20979 = CARTESIAN_POINT ( 'NONE',  ( -3.010752168931037698, 15.84372070116375575, -223.4060793985500482 ) ) ;
#20980 = ORIENTED_EDGE ( 'NONE', *, *, #7917, .T. ) ;
#20981 = CARTESIAN_POINT ( 'NONE',  ( 0.8374361358884788720, 23.73768315274483953, -232.4065959030912154 ) ) ;
#20982 = CARTESIAN_POINT ( 'NONE',  ( -24.92290506463145405, 6.124412323591598373, -220.3779252408000104 ) ) ;
#20983 = CARTESIAN_POINT ( 'NONE',  ( 26.75877786246624623, 11.80320999550499117, -231.5572967531201414 ) ) ;
#20984 = CARTESIAN_POINT ( 'NONE',  ( 6.869068212838696397, -24.78254998730118430, -231.2855974421026986 ) ) ;
#20985 = CARTESIAN_POINT ( 'NONE',  ( 20.13946171159960841, -0.1427001808266660232, -233.7987036390019853 ) ) ;
#20986 = CARTESIAN_POINT ( 'NONE',  ( 0.000000000000000000, 0.000000000000000000, -55.00000000000000000 ) ) ;
#20987 = CARTESIAN_POINT ( 'NONE',  ( 9.586902571418640662, 24.43292817174309661, -231.9968623198229807 ) ) ;
#20988 = CARTESIAN_POINT ( 'NONE',  ( -27.54101393026537181, -2.112662437277116556, -233.6092940012385384 ) ) ;
#20989 = DIRECTION ( 'NONE',  ( -0.000000000000000000, -0.000000000000000000, -1.000000000000000000 ) ) ;
#20990 = CARTESIAN_POINT ( 'NONE',  ( 15.01439307471096463, 1.118969480519667048, -226.7488225241675366 ) ) ;
#20991 = CARTESIAN_POINT ( 'NONE',  ( 1.623338700557370951, -21.82196275546919040, -234.1129525514646730 ) ) ;
#20992 = CARTESIAN_POINT ( 'NONE',  ( -18.70100282803782576, 16.58357028540773115, -216.4425743468854080 ) ) ;
#20993 = AXIS2_PLACEMENT_3D ( 'NONE', #6130, #11320, #16386 ) ;
#20994 = CARTESIAN_POINT ( 'NONE',  ( -12.39195900010699702, 23.13258866008456138, -233.4668451572263166 ) ) ;
#20995 = VERTEX_POINT ( 'NONE', #14250 ) ;
#20996 = CARTESIAN_POINT ( 'NONE',  ( -17.79285498209129202, 9.187865686019035749, -216.3798185811636756 ) ) ;
#20997 = CARTESIAN_POINT ( 'NONE',  ( -13.44605823798860200, -7.860403065310468840, -219.7865185367595586 ) ) ;
#20998 = CARTESIAN_POINT ( 'NONE',  ( -25.00000000000013500, -0.6682719527943432603, -10.00000000000000178 ) ) ;
#20999 = DIRECTION ( 'NONE',  ( 0.000000000000000000, 0.000000000000000000, -1.000000000000000000 ) ) ;
#21000 = CARTESIAN_POINT ( 'NONE',  ( -15.15434969228324924, 4.423874646950748613, -230.6144467931089821 ) ) ;
#21001 = CARTESIAN_POINT ( 'NONE',  ( 7.317916060359300978, -13.14109500694934951, -227.5371884182924305 ) ) ;
#21002 = CARTESIAN_POINT ( 'NONE',  ( 19.02418198972958407, -2.774848290582036636, -226.1609295929775669 ) ) ;
#21003 = CARTESIAN_POINT ( 'NONE',  ( 25.01541028746040141, 13.78427203520734423, -225.9266837950359843 ) ) ;
#21004 = CARTESIAN_POINT ( 'NONE',  ( -10.14083745617744547, 19.87482866967577877, -216.0596634563153486 ) ) ;
#21005 = DIRECTION ( 'NONE',  ( -0.000000000000000000, 0.000000000000000000, -1.000000000000000000 ) ) ;
#21006 = CARTESIAN_POINT ( 'NONE',  ( 10.32480721127626033, 15.84468581819879773, -230.0799086455579072 ) ) ;
#21007 = CARTESIAN_POINT ( 'NONE',  ( -0.8455829679720252567, -23.09678443543459991, -232.4899849032512122 ) ) ;
#21008 = EDGE_LOOP ( 'NONE', ( #10891, #10872, #21672, #21363 ) ) ;
#21009 = CARTESIAN_POINT ( 'NONE',  ( -11.03778527004271659, 26.96286968643956428, -225.4057095641571209 ) ) ;
#21010 = CARTESIAN_POINT ( 'NONE',  ( -8.892156391762910062, 11.89593067802204551, -225.4519868197583889 ) ) ;
#21011 = CARTESIAN_POINT ( 'NONE',  ( -21.12280458060320498, 13.61074013710079988, -216.5529903464332335 ) ) ;
#21012 = EDGE_LOOP ( 'NONE', ( #7845, #15119, #10788, #5121, #16761, #5512, #8211, #728, #5911, #6627, #15583, #8167, #435, #10808, #1019, #10343, #1783, #6769, #7035, #7769, #5430, #19325, #7657, #4404, #20332, #16293 ) ) ;
#21013 = PRESENTATION_LAYER_ASSIGNMENT (  '', '', ( #7000 ) ) ;
#21014 = CARTESIAN_POINT ( 'NONE',  ( -16.29786170208491924, -8.453292648900102790, -230.0691174225123632 ) ) ;
#21015 = DIRECTION ( 'NONE',  ( 1.000000000000000000, 0.000000000000000000, 0.000000000000000000 ) ) ;
#21016 = ORIENTED_EDGE ( 'NONE', *, *, #6596, .F. ) ;
#21017 = STYLED_ITEM ( 'NONE', ( #5582 ), #11503 ) ;
#21018 = CARTESIAN_POINT ( 'NONE',  ( -21.89065952084848021, -0.9940043559354364566, -216.9999999999999716 ) ) ;
#21019 = CARTESIAN_POINT ( 'NONE',  ( 7.144583572002897398, -18.19063289417396945, -230.4059351064080658 ) ) ;
#21020 = CARTESIAN_POINT ( 'NONE',  ( 20.23125423326388628, 7.836699765464857137, -217.8891354894872450 ) ) ;
#21021 = CARTESIAN_POINT ( 'NONE',  ( -10.51143808951550085, 11.41308718311005066, -231.3573069600382439 ) ) ;
#21022 = CARTESIAN_POINT ( 'NONE',  ( 27.79290571682592770, 12.05347838982552666, -230.1298045326732051 ) ) ;
#21023 = CARTESIAN_POINT ( 'NONE',  ( 12.04687593227112430, 27.54339840196571743, -224.6466266724203820 ) ) ;
#21024 = CARTESIAN_POINT ( 'NONE',  ( -17.50000000000007816, 0.000000000000000000, -55.00000000000000000 ) ) ;
#21025 = AXIS2_PLACEMENT_3D ( 'NONE', #7322, #14191, #664 ) ;
#21026 = CARTESIAN_POINT ( 'NONE',  ( -14.13781561609191328, -15.90667165809925621, -233.6615929499251649 ) ) ;
#21027 = AXIS2_PLACEMENT_3D ( 'NONE', #14137, #19292, #7591 ) ;
#21028 = CARTESIAN_POINT ( 'NONE',  ( 22.44368505003003378, -11.72633196808685163, -232.1179326287041533 ) ) ;
#21029 = CARTESIAN_POINT ( 'NONE',  ( 25.50000000000000000, 0.5000000000000000000, 0.000000000000000000 ) ) ;
#21030 = CARTESIAN_POINT ( 'NONE',  ( 0.000000000000000000, -17.50000000000000711, -30.00000000000000000 ) ) ;
#21031 = CARTESIAN_POINT ( 'NONE',  ( -10.54177647804913320, 7.401649028325941515, -220.3980514230326264 ) ) ;
#21032 = CARTESIAN_POINT ( 'NONE',  ( -17.17062072939792117, -6.705141685950851027, -229.6398969478225354 ) ) ;
#21033 = CARTESIAN_POINT ( 'NONE',  ( -24.18895665211001500, 11.26087434487096139, -231.0040666710689550 ) ) ;
#21034 = CARTESIAN_POINT ( 'NONE',  ( 21.77183241683778547, 12.04504704525620085, -233.6005549158834640 ) ) ;
#21035 = CARTESIAN_POINT ( 'NONE',  ( 5.446894657575932719, 15.00061806465251557, -226.4498309983864317 ) ) ;
#21036 = VERTEX_POINT ( 'NONE', #21083 ) ;
#21037 = CARTESIAN_POINT ( 'NONE',  ( 11.42868579270797369, -5.440147491673143598, -220.7688621915004603 ) ) ;
#21038 = CARTESIAN_POINT ( 'NONE',  ( 15.89706143421296147, 10.57416387607782227, -218.3862415393350318 ) ) ;
#21039 = CARTESIAN_POINT ( 'NONE',  ( -13.43384090552117271, 6.057765724406720231, -225.7182623230366119 ) ) ;
#21040 = CARTESIAN_POINT ( 'NONE',  ( -8.413706464639300719, 10.92140547936800843, -220.6417935981040728 ) ) ;
#21041 = CARTESIAN_POINT ( 'NONE',  ( -22.19673167533144564, -9.562764463827019057, -233.1557790568585062 ) ) ;
#21042 = CARTESIAN_POINT ( 'NONE',  ( -9.443239614166923701, 9.388015667058336788, -222.3195230688234290 ) ) ;
#21043 = DIRECTION ( 'NONE',  ( 1.224646799147353207E-16, 1.000000000000000000, 0.000000000000000000 ) ) ;
#21044 = CARTESIAN_POINT ( 'NONE',  ( 28.65393683769942967, 4.398063292302325067, -219.1542358361629965 ) ) ;
#21045 = CARTESIAN_POINT ( 'NONE',  ( -11.69222874857179484, 25.57550432052970280, -219.9467848335519591 ) ) ;
#21046 = CARTESIAN_POINT ( 'NONE',  ( 24.00840102751045890, 17.37402299239434100, -218.3110108534040137 ) ) ;
#21047 = CARTESIAN_POINT ( 'NONE',  ( -26.58771759052039485, 5.114955214121561511, -218.2823714869195442 ) ) ;
#21048 = CARTESIAN_POINT ( 'NONE',  ( -15.92941692657317354, -7.780888323563449838, -232.0381278758927976 ) ) ;
#21049 = CARTESIAN_POINT ( 'NONE',  ( 3.100794261777709782, 20.70580715608724276, -231.8781843337728219 ) ) ;
#21050 = CARTESIAN_POINT ( 'NONE',  ( -6.163092920833200594, -27.00835405423771007, -232.1022292408408987 ) ) ;
#21051 = CARTESIAN_POINT ( 'NONE',  ( 17.97843143658897347, 22.12221935793617078, -220.9346589834416079 ) ) ;
#21052 = CARTESIAN_POINT ( 'NONE',  ( 5.521532699605532279, -19.36944961733043513, -235.0341191922501594 ) ) ;
#21053 = AXIS2_PLACEMENT_3D ( 'NONE', #7127, #17248, #17359 ) ;
#21054 = DIRECTION ( 'NONE',  ( -1.000000000000000000, 0.000000000000000000, 0.000000000000000000 ) ) ;
#21055 = STYLED_ITEM ( 'NONE', ( #3371 ), #7772 ) ;
#21056 = CARTESIAN_POINT ( 'NONE',  ( 17.23039831256031817, 3.331158952577910615, -216.4027685342793461 ) ) ;
#21057 = DIRECTION ( 'NONE',  ( -1.000000000000000000, 0.000000000000000000, 0.000000000000000000 ) ) ;
#21058 = CARTESIAN_POINT ( 'NONE',  ( 27.81506808824343580, -10.52944849582878106, -221.0913368219556503 ) ) ;
#21059 = CARTESIAN_POINT ( 'NONE',  ( 10.64798096806036121, 19.48085866535796740, -231.3996658690317361 ) ) ;
#21060 = CARTESIAN_POINT ( 'NONE',  ( 29.81944548462877975, 8.043843257819576209, -228.1755181449411793 ) ) ;
#21061 = CARTESIAN_POINT ( 'NONE',  ( 17.07668571305246985, 2.037405138410691485, -219.7626854147787867 ) ) ;
#21062 = CARTESIAN_POINT ( 'NONE',  ( -7.007669255080013926, -23.60960382150139836, -233.3096631214588115 ) ) ;
#21063 =( REPRESENTATION_RELATIONSHIP ('NONE','NONE', #5277, #1546 ) REPRESENTATION_RELATIONSHIP_WITH_TRANSFORMATION ( #21981 )SHAPE_REPRESENTATION_RELATIONSHIP( ) );
#21064 = CARTESIAN_POINT ( 'NONE',  ( 11.31331191788792623, 29.23420701778062281, -220.7538464529627333 ) ) ;
#21065 = LINE ( 'NONE', #4185, #13398 ) ;
#21066 = CARTESIAN_POINT ( 'NONE',  ( -4.737391463177558215, -17.33199396152823368, -215.7912354007318925 ) ) ;
#21067 = CARTESIAN_POINT ( 'NONE',  ( -9.954421844142357756, 11.21484508112568079, -226.0177122452137439 ) ) ;
#21068 = CARTESIAN_POINT ( 'NONE',  ( 20.26651059498356844, 18.95255124124090074, -231.7206897233655525 ) ) ;
#21069 = CARTESIAN_POINT ( 'NONE',  ( -16.56270003954679382, 4.935922114544952777, -221.6503923146493378 ) ) ;
#21070 = CARTESIAN_POINT ( 'NONE',  ( 3.744112528862662881, 31.76296354843916703, -227.8872370379487506 ) ) ;
#21071 = CARTESIAN_POINT ( 'NONE',  ( 18.79638869589749461, 0.4878066561304963966, -219.5712168927955759 ) ) ;
#21072 = EDGE_CURVE ( 'NONE', #21666, #21036, #4302, .T. ) ;
#21073 = CARTESIAN_POINT ( 'NONE',  ( 13.80508996112396680, -23.93364289317450400, -226.6703843709330783 ) ) ;
#21074 = CARTESIAN_POINT ( 'NONE',  ( 12.20621255000322947, -21.57429421806300240, -232.1397031738524674 ) ) ;
#21075 = CARTESIAN_POINT ( 'NONE',  ( -0.2748333203896175525, 17.57683079704640505, -221.1444293135629948 ) ) ;
#21076 = EDGE_LOOP ( 'NONE', ( #179, #10918, #20558, #2613 ) ) ;
#21077 = DIRECTION ( 'NONE',  ( 0.000000000000000000, 0.000000000000000000, -1.000000000000000000 ) ) ;
#21078 = CARTESIAN_POINT ( 'NONE',  ( 17.34727976380017722, 4.822939981779328811, -230.8836217450937909 ) ) ;
#21079 = CARTESIAN_POINT ( 'NONE',  ( 16.08921376350389920, -2.840750994787607731, -229.5571464835293796 ) ) ;
#21080 = CARTESIAN_POINT ( 'NONE',  ( -13.88883449434014672, -11.15328429608096172, -217.8357414694029046 ) ) ;
#21081 = CARTESIAN_POINT ( 'NONE',  ( -8.376153411442972541, -27.59911039556260448, -219.0729038785590888 ) ) ;
#21082 = CARTESIAN_POINT ( 'NONE',  ( -7.770318051073092036, 21.02940971564074957, -231.8751410922876630 ) ) ;
#21083 = CARTESIAN_POINT ( 'NONE',  ( 21.50000000000000711, 2.632990618166810418E-15, -55.00000000000000711 ) ) ;
#21084 = CARTESIAN_POINT ( 'NONE',  ( 15.99247752609008444, 10.72268246046808216, -230.5614800526110173 ) ) ;
#21085 = CARTESIAN_POINT ( 'NONE',  ( -6.855867220396999251, 12.17758473459128332, -220.6375607554995213 ) ) ;
#21086 = CARTESIAN_POINT ( 'NONE',  ( -11.11479000491124047, 20.76372272540567110, -218.2001872134434564 ) ) ;
#21087 = VERTEX_POINT ( 'NONE', #18382 ) ;
#21088 = ORIENTED_EDGE ( 'NONE', *, *, #2109, .T. ) ;
#21089 = CARTESIAN_POINT ( 'NONE',  ( 2.471164685565028662, 14.01327037412690935, -223.4905256513065410 ) ) ;
#21090 = CARTESIAN_POINT ( 'NONE',  ( 17.91327661571172314, 1.545939370248587075, -216.9938266089438912 ) ) ;
#21091 = CARTESIAN_POINT ( 'NONE',  ( 17.98589043827631428, 2.945998030785370592, -233.4030907785035538 ) ) ;
#21092 = ADVANCED_FACE ( 'NONE', ( #1275 ), #14903, .T. ) ;
#21093 = CARTESIAN_POINT ( 'NONE',  ( 6.930886114109415352, -28.33506752827666020, -226.0544877841801110 ) ) ;
#21094 = DIRECTION ( 'NONE',  ( -0.000000000000000000, -0.000000000000000000, -1.000000000000000000 ) ) ;
#21095 = ORIENTED_EDGE ( 'NONE', *, *, #18214, .T. ) ;
#21096 = CARTESIAN_POINT ( 'NONE',  ( 2.837900457371055563, 25.11342719071438978, -232.9871906064174709 ) ) ;
#21097 = CARTESIAN_POINT ( 'NONE',  ( 17.01404819207892061, -3.492736430306117690, -221.2516733069050190 ) ) ;
#21098 = DIRECTION ( 'NONE',  ( -0.000000000000000000, 0.000000000000000000, -1.000000000000000000 ) ) ;
#21099 = EDGE_CURVE ( 'NONE', #19867, #19741, #15303, .T. ) ;
#21100 = CARTESIAN_POINT ( 'NONE',  ( 6.589392574981438599, -17.08498810221841069, -232.9613445306918322 ) ) ;
#21101 = CARTESIAN_POINT ( 'NONE',  ( -12.74846050492543625, 19.93509882904884734, -216.0172840992881049 ) ) ;
#21102 = CARTESIAN_POINT ( 'NONE',  ( -13.24620988741752825, 28.78239319002125285, -225.3527830703614256 ) ) ;
#21103 = ORIENTED_EDGE ( 'NONE', *, *, #8010, .T. ) ;
#21104 = CARTESIAN_POINT ( 'NONE',  ( -9.740348021262962064, 16.12529029871877384, -216.4361617420699702 ) ) ;
#21105 = CARTESIAN_POINT ( 'NONE',  ( -12.18037021406049547, -6.685450889859271051, -226.7642181357440734 ) ) ;
#21106 = CARTESIAN_POINT ( 'NONE',  ( 1.665334536937734811E-13, -23.00000000000000000, 69.99999999999998579 ) ) ;
#21107 = CARTESIAN_POINT ( 'NONE',  ( -22.03299105905330535, 6.604150919132904640, -7.515967719178155981 ) ) ;
#21108 = CARTESIAN_POINT ( 'NONE',  ( -25.29098058636142810, 5.014641116111857144, -217.4658967307323110 ) ) ;
#21109 = CARTESIAN_POINT ( 'NONE',  ( 10.12607331509846986, -17.07097861414113638, -217.9029769802564545 ) ) ;
#21110 = CARTESIAN_POINT ( 'NONE',  ( 14.40511183577193677, -1.529481993174749865, -222.4191515927619776 ) ) ;
#21111 = CARTESIAN_POINT ( 'NONE',  ( -18.09776816382430908, 23.50806826204562583, -229.9568677523880638 ) ) ;
#21112 = CARTESIAN_POINT ( 'NONE',  ( 12.51085646230496273, 9.582567546749562126, -224.6200301875240939 ) ) ;
#21113 = CARTESIAN_POINT ( 'NONE',  ( -23.16143087541734502, 21.36835206473086046, -221.8715256527013651 ) ) ;
#21114 = CARTESIAN_POINT ( 'NONE',  ( 13.62455467724876712, 0.2254024858538909992, -227.9921160535819809 ) ) ;
#21115 = CARTESIAN_POINT ( 'NONE',  ( 20.64430047260004031, 12.67811357335941480, -231.0449411089858813 ) ) ;
#21116 = CARTESIAN_POINT ( 'NONE',  ( 5.229904874806564408, -24.29892824652383609, -233.0630010234598046 ) ) ;
#21117 = ORIENTED_EDGE ( 'NONE', *, *, #11520, .T. ) ;
#21118 = CARTESIAN_POINT ( 'NONE',  ( 3.367418898937407867, 27.20023797116225595, -219.3349021808245709 ) ) ;
#21119 = CARTESIAN_POINT ( 'NONE',  ( -10.65640919150578192, 23.79238421564942740, -218.1088542024188826 ) ) ;
#21120 = CARTESIAN_POINT ( 'NONE',  ( 21.43345597994050777, 2.294722475943265838, -232.7243927205661294 ) ) ;
#21121 = CARTESIAN_POINT ( 'NONE',  ( -11.98587399847077783, -10.70615994290841044, -225.3229167341726225 ) ) ;
#21122 = DIRECTION ( 'NONE',  ( -0.000000000000000000, -0.000000000000000000, 1.000000000000000000 ) ) ;
#21123 = EDGE_LOOP ( 'NONE', ( #1673, #5881, #6941, #5234 ) ) ;
#21124 = CARTESIAN_POINT ( 'NONE',  ( 24.32561047128371001, 1.769413244618101011, -218.8629106451077462 ) ) ;
#21125 = CARTESIAN_POINT ( 'NONE',  ( 0.7938325546108213615, -23.90362011959725663, -218.0438616059182380 ) ) ;
#21126 = CARTESIAN_POINT ( 'NONE',  ( 16.84848658399567611, 11.39632653812981644, -217.9589513831453473 ) ) ;
#21127 = CARTESIAN_POINT ( 'NONE',  ( -2.698926868850080041, 12.89339462271858316, -226.7595176699009585 ) ) ;
#21128 = UNCERTAINTY_MEASURE_WITH_UNIT (LENGTH_MEASURE( 1.000000000000000082E-05 ), #8197, 'distance_accuracy_value', 'NONE');
#21129 = CARTESIAN_POINT ( 'NONE',  ( -16.08005950484750102, -0.1764640578214327904, -223.5999988222837942 ) ) ;
#21130 = CARTESIAN_POINT ( 'NONE',  ( 3.449504654906655254, 27.59247159270940841, -231.3461799890608859 ) ) ;
#21131 = CARTESIAN_POINT ( 'NONE',  ( 14.95656649340767430, 1.888692170932965597, -222.6673885184368089 ) ) ;
#21132 = CARTESIAN_POINT ( 'NONE',  ( -14.34280792637948743, -22.10828917559366147, -217.4172704053049756 ) ) ;
#21133 = CARTESIAN_POINT ( 'NONE',  ( 13.04434844185555420, -10.19049307777131297, -230.8679447648462713 ) ) ;
#21134 = CYLINDRICAL_SURFACE ( 'NONE', #13491, 17.50000000000000711 ) ;
#21135 = DIRECTION ( 'NONE',  ( 0.000000000000000000, 0.000000000000000000, -1.000000000000000000 ) ) ;
#21136 = CARTESIAN_POINT ( 'NONE',  ( -12.02603758797190459, 8.152912069735307909, -218.2257190893353709 ) ) ;
#21137 = CARTESIAN_POINT ( 'NONE',  ( -24.19871179313096476, -3.348666575842360160, -230.4488973568908534 ) ) ;
#21138 = CARTESIAN_POINT ( 'NONE',  ( -21.19360951076126653, 12.15251088906093457, -217.9482185194656552 ) ) ;
#21139 = CARTESIAN_POINT ( 'NONE',  ( 17.29648694364601980, 10.20782262162153842, -233.8400727604031317 ) ) ;
#21140 = CARTESIAN_POINT ( 'NONE',  ( -1.565160934061885500, 18.19073094521525391, -232.0278805765578909 ) ) ;
#21141 = EDGE_LOOP ( 'NONE', ( #15963, #11315, #12691, #15157, #19168, #18752 ) ) ;
#21142 = CARTESIAN_POINT ( 'NONE',  ( 26.81360599170068326, -17.93330511230891844, -224.0089312182945491 ) ) ;
#21143 = CARTESIAN_POINT ( 'NONE',  ( 17.00168025137501004, 6.212099629982537508, -219.0548246536471595 ) ) ;
#21144 = CARTESIAN_POINT ( 'NONE',  ( -0.8357710952364670876, 15.48480697989137234, -216.9118565312697910 ) ) ;
#21145 = CARTESIAN_POINT ( 'NONE',  ( -4.678665819194652187, 12.50541869316310262, -220.1509054161798247 ) ) ;
#21146 = CARTESIAN_POINT ( 'NONE',  ( -13.63272521699743756, -3.226083955879493814, -228.1383267723209656 ) ) ;
#21147 = CARTESIAN_POINT ( 'NONE',  ( -9.540790481621398200, 9.981116473660406996, -228.6478862620407995 ) ) ;
#21148 = CIRCLE ( 'NONE', #19710, 23.00000000000008882 ) ;
#21149 = DIRECTION ( 'NONE',  ( 1.000000000000000000, 0.000000000000000000, -0.000000000000000000 ) ) ;
#21150 = CARTESIAN_POINT ( 'NONE',  ( 19.63495056682994289, -4.096126682090319271, -232.1271738766904207 ) ) ;
#21151 = CARTESIAN_POINT ( 'NONE',  ( -21.10507617219916199, 14.90539259013048756, -229.7677326419877488 ) ) ;
#21152 = CARTESIAN_POINT ( 'NONE',  ( -16.90857133559978465, -0.4126725064255206687, -221.6276144895144569 ) ) ;
#21153 = CARTESIAN_POINT ( 'NONE',  ( -14.68037037322036475, 3.441677802729143920, -220.1396515630443389 ) ) ;
#21154 = CARTESIAN_POINT ( 'NONE',  ( 4.907833106823921376, 13.98151846258800290, -229.0190609869640923 ) ) ;
#21155 = CARTESIAN_POINT ( 'NONE',  ( -26.09107693309126574, -10.38942742183557399, -230.9365759677854442 ) ) ;
#21156 = CARTESIAN_POINT ( 'NONE',  ( 4.482815116226093188, 26.97722808566452812, -229.2080185206130238 ) ) ;
#21157 = CARTESIAN_POINT ( 'NONE',  ( -5.240862053303020573, -11.96147391800445270, -224.1453450823045443 ) ) ;
#21158 = CARTESIAN_POINT ( 'NONE',  ( 5.141746912158045468, 22.01688500372448232, -216.6678693612369386 ) ) ;
#21159 = CARTESIAN_POINT ( 'NONE',  ( 17.14704237169575052, -19.77033640698606121, -215.4809218419665342 ) ) ;
#21160 = CARTESIAN_POINT ( 'NONE',  ( 13.91172867693016890, -0.1003083830847898567, -227.9999999999999147 ) ) ;
#21161 = EDGE_CURVE ( 'NONE', #13588, #20089, #211, .T. ) ;
#21162 = CARTESIAN_POINT ( 'NONE',  ( -10.30870167223346456, 11.95603877111467561, -228.4123369090513336 ) ) ;
#21163 = DIRECTION ( 'NONE',  ( -1.000000000000000000, -0.000000000000000000, -0.000000000000000000 ) ) ;
#21164 = CARTESIAN_POINT ( 'NONE',  ( 23.33467929415965614, -0.4823873731835089940, -233.9427286327415629 ) ) ;
#21165 = CARTESIAN_POINT ( 'NONE',  ( 3.689800395305025127, 23.07294874520714956, -219.2515233573129478 ) ) ;
#21166 = CARTESIAN_POINT ( 'NONE',  ( -20.47640197314466093, 18.50423766437512541, -220.4440130802851456 ) ) ;
#21167 = CARTESIAN_POINT ( 'NONE',  ( -19.86079186537285324, -0.7838168488858909821, -215.1601656726509475 ) ) ;
#21168 = CARTESIAN_POINT ( 'NONE',  ( -15.89829452305285606, -16.08449805557013335, -231.9408725418336701 ) ) ;
#21169 = CARTESIAN_POINT ( 'NONE',  ( 19.49137065790598555, 9.165486118354671419, -234.8706749352814995 ) ) ;
#21170 = FACE_OUTER_BOUND ( 'NONE', #1801, .T. ) ;
#21171 = CARTESIAN_POINT ( 'NONE',  ( -0.6133843921297743584, -15.86829592205942419, -231.9438830533787268 ) ) ;
#21172 = CARTESIAN_POINT ( 'NONE',  ( 3.219568897812384645, 28.82511222849302257, -221.5626884747494216 ) ) ;
#21173 = CARTESIAN_POINT ( 'NONE',  ( 10.49811526528768368, 13.26166588535847701, -217.9009921269571919 ) ) ;
#21174 = CARTESIAN_POINT ( 'NONE',  ( -12.70465517376339193, 12.03139199664008530, -229.6235454691090752 ) ) ;
#21175 = ADVANCED_BREP_SHAPE_REPRESENTATION ( '', ( #14295, #6677 ), #10247 ) ;
#21176 = AXIS2_PLACEMENT_3D ( 'NONE', #3767, #12778, #10863 ) ;
#21177 = CARTESIAN_POINT ( 'NONE',  ( -0.4465333940385243228, 12.27026616490476485, -221.3722328744566425 ) ) ;
#21178 = CARTESIAN_POINT ( 'NONE',  ( 13.14260364752544596, 5.866423290307341887, -222.7705901084601408 ) ) ;
#21179 = EDGE_LOOP ( 'NONE', ( #17748, #14675, #11334, #3819 ) ) ;
#21180 = CARTESIAN_POINT ( 'NONE',  ( 10.07328213880649592, -15.27579949576245966, -229.4560222226588451 ) ) ;
#21181 = CARTESIAN_POINT ( 'NONE',  ( 7.680972971696337304, -18.49313070787806623, -217.8811398819712508 ) ) ;
#21182 = CARTESIAN_POINT ( 'NONE',  ( -3.504118661534079582, 16.69899759879061918, -221.4378787282527128 ) ) ;
#21183 = FACE_OUTER_BOUND ( 'NONE', #5480, .T. ) ;
#21184 = CARTESIAN_POINT ( 'NONE',  ( 21.53262694368047647, 11.06794636811408594, -231.8394491640143826 ) ) ;
#21185 = CARTESIAN_POINT ( 'NONE',  ( 16.06750045776299629, -1.909440863493336860, -220.4398626676318713 ) ) ;
#21186 = CARTESIAN_POINT ( 'NONE',  ( -13.72709560065558421, -5.132649126379569715, -227.9317987811764965 ) ) ;
#21187 = CARTESIAN_POINT ( 'NONE',  ( 2.098184199980985376, -13.29281380427311099, -222.1652846463370281 ) ) ;
#21188 = EDGE_CURVE ( 'NONE', #5788, #15541, #17465, .T. ) ;
#21189 = CARTESIAN_POINT ( 'NONE',  ( 6.729623925010410623, 16.84721552001897038, -219.9221131804260381 ) ) ;
#21190 = DIRECTION ( 'NONE',  ( -0.000000000000000000, -0.000000000000000000, 1.000000000000000000 ) ) ;
#21191 = CARTESIAN_POINT ( 'NONE',  ( 19.10353041285295816, 2.510539514498965730, -232.1135168369976896 ) ) ;
#21192 = CARTESIAN_POINT ( 'NONE',  ( -9.716674560061926869, 27.56227806819028103, -219.4917914922789919 ) ) ;
#21193 = CARTESIAN_POINT ( 'NONE',  ( 5.688640247940316641, 20.34961083808282822, -230.9155060479073711 ) ) ;
#21194 = EDGE_LOOP ( 'NONE', ( #6878, #10449, #12623, #10956 ) ) ;
#21195 = CARTESIAN_POINT ( 'NONE',  ( 15.37089934297015503, 20.64239674606488961, -217.2018742121147170 ) ) ;
#21196 = CARTESIAN_POINT ( 'NONE',  ( -16.45414350258782221, 17.57852913985137988, -231.3969631806205598 ) ) ;
#21197 = CARTESIAN_POINT ( 'NONE',  ( 14.81258087342262364, 2.398747990731791013, -230.9000679928271040 ) ) ;
#21198 = CARTESIAN_POINT ( 'NONE',  ( 2.641673488600395636, -17.65289918763021149, -219.1873688300129288 ) ) ;
#21199 = DIRECTION ( 'NONE',  ( -1.000000000000000000, 0.000000000000000000, 0.000000000000000000 ) ) ;
#21200 = CARTESIAN_POINT ( 'NONE',  ( 0.000000000000000000, 0.000000000000000000, -75.00000000000000000 ) ) ;
#21201 = EDGE_CURVE ( 'NONE', #2791, #17378, #20675, .T. ) ;
#21202 = CARTESIAN_POINT ( 'NONE',  ( 11.82943521288609823, 27.58963564415041247, -226.1180395413371400 ) ) ;
#21203 = CARTESIAN_POINT ( 'NONE',  ( -29.11561446909439965, 0.2226424683783513325, -217.8829860219008765 ) ) ;
#21204 = FACE_OUTER_BOUND ( 'NONE', #16382, .T. ) ;
#21205 = CARTESIAN_POINT ( 'NONE',  ( -0.6367083786117293531, -29.73461014436635708, -220.1383336929387724 ) ) ;
#21206 = APPLICATION_PROTOCOL_DEFINITION ( 'draft international standard', 'automotive_design', 1998, #3384 ) ;
#21207 = CARTESIAN_POINT ( 'NONE',  ( -17.75316132689678383, 25.03468689048078843, -222.1645193425721061 ) ) ;
#21208 = CARTESIAN_POINT ( 'NONE',  ( -6.111257124579617894, 15.89946952501658295, -216.3497764690875727 ) ) ;
#21209 = VERTEX_POINT ( 'NONE', #15014 ) ;
#21210 = CARTESIAN_POINT ( 'NONE',  ( -11.49049084071896409, 11.06834963248926940, -218.3354249205727058 ) ) ;
#21211 = CARTESIAN_POINT ( 'NONE',  ( -21.14773328851117995, -13.15959238732831693, -217.2646803791660943 ) ) ;
#21212 = DIRECTION ( 'NONE',  ( -1.000000000000000000, 0.000000000000000000, 0.000000000000000000 ) ) ;
#21213 = CARTESIAN_POINT ( 'NONE',  ( -22.56530582151367170, 4.460126506072113806, -8.956185171266239919 ) ) ;
#21214 = CARTESIAN_POINT ( 'NONE',  ( -10.45786516112131892, 23.61456281964591852, -233.2869923610001592 ) ) ;
#21215 = CARTESIAN_POINT ( 'NONE',  ( 6.466495776945791363, -21.72297233841655029, -216.6235280138562302 ) ) ;
#21216 = DIRECTION ( 'NONE',  ( -1.000000000000000000, 0.000000000000000000, 0.000000000000000000 ) ) ;
#21217 = CARTESIAN_POINT ( 'NONE',  ( -27.90314475660494153, 12.48829126175061077, -223.3300566725355338 ) ) ;
#21218 = CARTESIAN_POINT ( 'NONE',  ( 14.65309016725241698, 3.424799466898550637, -221.5217808432381048 ) ) ;
#21219 = CARTESIAN_POINT ( 'NONE',  ( 2.208705534715813101, 15.26926593729510984, -227.3643075380122980 ) ) ;
#21220 = DIRECTION ( 'NONE',  ( 0.000000000000000000, 0.000000000000000000, -1.000000000000000000 ) ) ;
#21221 = CARTESIAN_POINT ( 'NONE',  ( 14.02802030611117878, 3.063901161068346646, -225.6350222114233475 ) ) ;
#21222 = CARTESIAN_POINT ( 'NONE',  ( -17.99186107021003167, -20.03292934477192944, -228.1636640080403424 ) ) ;
#21223 = VERTEX_POINT ( 'NONE', #7704 ) ;
#21224 = CARTESIAN_POINT ( 'NONE',  ( 3.291078285693179950, 23.55624334554876498, -217.3208248278388623 ) ) ;
#21225 = CARTESIAN_POINT ( 'NONE',  ( -18.67270963783218463, 15.11229250701181925, -218.9067109956068578 ) ) ;
#21226 = CARTESIAN_POINT ( 'NONE',  ( -8.221702953833418093, 11.87876791566348800, -223.9138461338794741 ) ) ;
#21227 = CARTESIAN_POINT ( 'NONE',  ( -9.669661339602258820, -12.96780954771633532, -224.3029626631937106 ) ) ;
#21228 = CARTESIAN_POINT ( 'NONE',  ( 1.317067778529001989E-13, -19.63401512838754215, -77.51594804401857175 ) ) ;
#21229 = EDGE_LOOP ( 'NONE', ( #9, #19057 ) ) ;
#21230 = CARTESIAN_POINT ( 'NONE',  ( -16.20072894238734307, 0.5024448614660336210, -230.4554067149722130 ) ) ;
#21231 = CARTESIAN_POINT ( 'NONE',  ( 7.513872959756128012, -15.38293111518118295, -221.6143039513618760 ) ) ;
#21232 = CARTESIAN_POINT ( 'NONE',  ( 13.03557269046774714, 7.519834803053426775, -226.9490612297269081 ) ) ;
#21233 = CARTESIAN_POINT ( 'NONE',  ( -2.772442535524381579, 13.75675912271027457, -228.9770533867650215 ) ) ;
#21234 = CARTESIAN_POINT ( 'NONE',  ( -25.94982248293519689, 10.67899231259548287, -221.1273147719203962 ) ) ;
#21235 = CARTESIAN_POINT ( 'NONE',  ( 14.02309809840729393, 19.05079204846204277, -234.6885355850075143 ) ) ;
#21236 = EDGE_CURVE ( 'NONE', #1916, #10146, #21392, .T. ) ;
#21237 = CARTESIAN_POINT ( 'NONE',  ( 13.49011766416699842, 7.659170998773840111, -228.1905628957712793 ) ) ;
#21238 = DIRECTION ( 'NONE',  ( 0.000000000000000000, 0.000000000000000000, -1.000000000000000000 ) ) ;
#21239 = CARTESIAN_POINT ( 'NONE',  ( -13.88883449434014672, -11.15328429608096172, -217.8357414694029046 ) ) ;
#21240 = CARTESIAN_POINT ( 'NONE',  ( 1.904360901363437275, -12.77109371939166138, -224.5066922355585177 ) ) ;
#21241 = CARTESIAN_POINT ( 'NONE',  ( 0.000000000000000000, 21.00000000000006395, 75.00000000000000000 ) ) ;
#21242 = LINE ( 'NONE', #5834, #1190 ) ;
#21243 = CARTESIAN_POINT ( 'NONE',  ( -11.79271689233719478, 3.876813423829604144, -228.6816298097564299 ) ) ;
#21244 = CARTESIAN_POINT ( 'NONE',  ( 24.04182214053767908, -5.779968796880146975, -234.9365023861272164 ) ) ;
#21245 = CARTESIAN_POINT ( 'NONE',  ( 5.833753951408669813, 12.47745132051510453, -226.2508980627489450 ) ) ;
#21246 = CARTESIAN_POINT ( 'NONE',  ( 6.685304925496912354, 17.61973327427626046, -230.4152170797364931 ) ) ;
#21247 = ORIENTED_EDGE ( 'NONE', *, *, #9702, .T. ) ;
#21248 = CARTESIAN_POINT ( 'NONE',  ( 6.498966860804143764, -11.65341448970024274, -221.3944939044252749 ) ) ;
#21249 = CARTESIAN_POINT ( 'NONE',  ( 25.80927844399814930, 11.21489550116160316, -221.3538377621514996 ) ) ;
#21250 = AXIS2_PLACEMENT_3D ( 'NONE', #16850, #15495, #22241 ) ;
#21251 = CARTESIAN_POINT ( 'NONE',  ( -4.155456637169709921, 11.30291311430030987, -225.2606024264729001 ) ) ;
#21252 = CARTESIAN_POINT ( 'NONE',  ( -4.845359737286285551, 16.85396349487340117, -233.9229833851842670 ) ) ;
#21253 = CARTESIAN_POINT ( 'NONE',  ( -27.06419889410506485, -1.187659473326917237, -217.6367138431444630 ) ) ;
#21254 = CARTESIAN_POINT ( 'NONE',  ( -16.39453490553961856, 20.24836633112041184, -233.1722131570092245 ) ) ;
#21255 = CARTESIAN_POINT ( 'NONE',  ( -10.29801091644274713, -10.20851360429410803, 92.99999999999998579 ) ) ;
#21256 = CARTESIAN_POINT ( 'NONE',  ( 27.92729748684602598, -8.572309054117944527, -222.6487661343338686 ) ) ;
#21257 = AXIS2_PLACEMENT_3D ( 'NONE', #9728, #20164, #8048 ) ;
#21258 = CARTESIAN_POINT ( 'NONE',  ( -4.021035526861677312, 25.02763064454595110, -216.6167103172201678 ) ) ;
#21259 = CARTESIAN_POINT ( 'NONE',  ( 25.70350299105564318, 4.008313962570879241, -233.1578316763087173 ) ) ;
#21260 = CARTESIAN_POINT ( 'NONE',  ( -16.63766460830045091, 5.158675778507696208, -232.1659425527909093 ) ) ;
#21261 = CARTESIAN_POINT ( 'NONE',  ( 10.66614775643814994, 26.29080367171353672, -230.0818785118670178 ) ) ;
#21262 = CARTESIAN_POINT ( 'NONE',  ( 1.526556658859590748E-13, -21.00000000000006395, 75.00000000000000000 ) ) ;
#21263 = CARTESIAN_POINT ( 'NONE',  ( -4.211886032913159106, 20.62037006687756602, -216.9488349035050305 ) ) ;
#21264 = CARTESIAN_POINT ( 'NONE',  ( -13.05629324012484282, -10.24599397043673221, -218.7452066004821347 ) ) ;
#21265 = CARTESIAN_POINT ( 'NONE',  ( 10.50530447320976535, 20.19629329636330084, -217.1354359361034767 ) ) ;
#21266 = CARTESIAN_POINT ( 'NONE',  ( 7.391697205318404684, -9.868666992833734497, -221.1858763705714068 ) ) ;
#21267 = DIRECTION ( 'NONE',  ( -0.000000000000000000, -0.000000000000000000, -1.000000000000000000 ) ) ;
#21268 = VECTOR ( 'NONE', #20021, 1000.000000000000000 ) ;
#21269 = CARTESIAN_POINT ( 'NONE',  ( -12.06153928353927540, 8.661506524875534296, -226.8425068572842349 ) ) ;
#21270 = SURFACE_STYLE_USAGE ( .BOTH. , #19371 ) ;
#21271 = CARTESIAN_POINT ( 'NONE',  ( 24.68983475587330645, -0.6584631617853404784, -233.6195837498767958 ) ) ;
#21272 = CARTESIAN_POINT ( 'NONE',  ( 2.021807401899061496, 24.17554150923399092, -230.4042646614662146 ) ) ;
#21273 = CARTESIAN_POINT ( 'NONE',  ( -13.97943781666340790, 5.798109546139844639, -228.2992319913466019 ) ) ;
#21274 = CARTESIAN_POINT ( 'NONE',  ( -13.09048442463468120, -0.002406630494250819839, -229.7150300986316438 ) ) ;
#21275 = CARTESIAN_POINT ( 'NONE',  ( -17.60926409178586738, -17.65542935640887023, -231.2676365506119680 ) ) ;
#21276 = CARTESIAN_POINT ( 'NONE',  ( 13.34963947135311102, 7.416462695144936390, -217.9359469527792044 ) ) ;
#21277 = LINE ( 'NONE', #12750, #19157 ) ;
#21278 = CARTESIAN_POINT ( 'NONE',  ( -16.38285517717123341, -14.67507636997927989, -214.6561055496966901 ) ) ;
#21279 = CARTESIAN_POINT ( 'NONE',  ( 0.8374361358884788720, 23.73768315274483953, -232.4065959030912154 ) ) ;
#21280 = CARTESIAN_POINT ( 'NONE',  ( 13.93840998928060415, 0.7705246578886114639, -220.8158265847476116 ) ) ;
#21281 = CIRCLE ( 'NONE', #6208, 3.000000000000002665 ) ;
#21282 = CARTESIAN_POINT ( 'NONE',  ( -14.22959263369750182, 18.28478771081826793, -217.8090497856120464 ) ) ;
#21283 = CARTESIAN_POINT ( 'NONE',  ( -1.584125552723561592, 20.48724127025963782, -214.7515060525244621 ) ) ;
#21284 = CARTESIAN_POINT ( 'NONE',  ( -17.96792326766206926, -0.6237852504629022299, -217.9759415197746932 ) ) ;
#21285 = CARTESIAN_POINT ( 'NONE',  ( -4.832117640292445060, -22.41582585812286865, -216.8192401332019870 ) ) ;
#21286 = CARTESIAN_POINT ( 'NONE',  ( 15.69671663880151868, -19.77919342852767315, -217.9503656454650411 ) ) ;
#21287 = CARTESIAN_POINT ( 'NONE',  ( -21.63401512838748175, 2.649402737968514273E-15, -77.51594804401857175 ) ) ;
#21288 = CARTESIAN_POINT ( 'NONE',  ( 24.42567939027770407, 10.22651298688739097, -219.4562066833365748 ) ) ;
#21289 = CARTESIAN_POINT ( 'NONE',  ( -24.78158512205813224, 1.917202307505101455, -217.2232489266994833 ) ) ;
#21290 = CARTESIAN_POINT ( 'NONE',  ( -9.294226473174397540, -12.00440878504259601, -219.6990993854437875 ) ) ;
#21291 = CARTESIAN_POINT ( 'NONE',  ( -18.44715843167851688, -19.86029123650958184, -231.9563062773970046 ) ) ;
#21292 = CARTESIAN_POINT ( 'NONE',  ( 5.688640247940316641, 20.34961083808282822, -230.9155060479073711 ) ) ;
#21293 = CARTESIAN_POINT ( 'NONE',  ( 0.000000000000000000, 0.000000000000000000, -126.0000000000000284 ) ) ;
#21294 = CARTESIAN_POINT ( 'NONE',  ( -13.34869474643618581, 6.516017165032126357, -231.2228057326931321 ) ) ;
#21295 = CARTESIAN_POINT ( 'NONE',  ( -15.58461825850822180, 18.91734573546571951, -233.7691177939990723 ) ) ;
#21296 = CARTESIAN_POINT ( 'NONE',  ( 6.136979247480394584, 21.37054498543370684, -230.9985475420231467 ) ) ;
#21297 = CARTESIAN_POINT ( 'NONE',  ( 29.03861746756086859, -6.579333063807603743, -229.8282242506458317 ) ) ;
#21298 = EDGE_LOOP ( 'NONE', ( #20587, #1914, #4519, #16716 ) ) ;
#21299 = CIRCLE ( 'NONE', #8023, 3.000000000000002665 ) ;
#21300 = CARTESIAN_POINT ( 'NONE',  ( 8.592982993077152187, 10.20906991731218838, -226.0923132092261483 ) ) ;
#21301 = CARTESIAN_POINT ( 'NONE',  ( -18.09605518090995702, 22.22778748761825085, -222.5443354630425290 ) ) ;
#21302 = CARTESIAN_POINT ( 'NONE',  ( 29.96674103997387206, 4.060923908484647349, -228.5323681967686298 ) ) ;
#21303 = CARTESIAN_POINT ( 'NONE',  ( 0.9095753368782393267, -25.50589708844611891, -231.1945442011520697 ) ) ;
#21304 = DIRECTION ( 'NONE',  ( -1.000000000000000000, 0.000000000000000000, 0.000000000000000000 ) ) ;
#21305 = VERTEX_POINT ( 'NONE', #8149 ) ;
#21306 = CARTESIAN_POINT ( 'NONE',  ( 9.107417252317809186, 16.30291009569977234, -218.0131178633739921 ) ) ;
#21307 = CARTESIAN_POINT ( 'NONE',  ( 13.24102317311734112, -10.11186274821533715, -227.6843928184991057 ) ) ;
#21308 = CARTESIAN_POINT ( 'NONE',  ( -28.31595744342370580, 5.786754998807587924, -229.0820962600229223 ) ) ;
#21309 = CARTESIAN_POINT ( 'NONE',  ( -2.270280637033633475, -14.48864307936496765, -230.4581659391201072 ) ) ;
#21310 = APPLICATION_PROTOCOL_DEFINITION ( 'draft international standard', 'automotive_design', 1998, #7149 ) ;
#21311 = CARTESIAN_POINT ( 'NONE',  ( 4.340445191644851874, 29.86837761166362881, -227.4879512554873315 ) ) ;
#21313 = CARTESIAN_POINT ( 'NONE',  ( 6.839751633953758514, 19.11639828585652623, -235.1218211620789873 ) ) ;
#21312 = AXIS2_PLACEMENT_3D ( 'NONE', #8084, #16852, #6606 ) ;
#21314 = ORIENTED_EDGE ( 'NONE', *, *, #1150, .F. ) ;
#21315 = CARTESIAN_POINT ( 'NONE',  ( -24.24202834850560606, 19.05981756344202438, -226.6980666352953335 ) ) ;
#21316 = CARTESIAN_POINT ( 'NONE',  ( 29.05460218321669785, -4.534277981440765437, -222.0637325791020373 ) ) ;
#21317 = AXIS2_PLACEMENT_3D ( 'NONE', #19528, #4114, #12791 ) ;
#21318 = CARTESIAN_POINT ( 'NONE',  ( 0.000000000000000000, 0.000000000000000000, -60.00000000000000000 ) ) ;
#21319 = DIRECTION ( 'NONE',  ( 1.000000000000000000, 0.000000000000000000, 0.000000000000000000 ) ) ;
#21320 = CARTESIAN_POINT ( 'NONE',  ( -8.966714183099560032, 19.05224306381768073, -234.0879867025980445 ) ) ;
#21321 = MANIFOLD_SOLID_BREP ( 'Revolve1', #20845 ) ;
#21322 = CARTESIAN_POINT ( 'NONE',  ( 8.082980660592431477, -16.66562551544545201, -231.4954396659114764 ) ) ;
#21324 = EDGE_CURVE ( 'NONE', #11616, #4018, #3420, .T. ) ;
#21323 = DIRECTION ( 'NONE',  ( 0.000000000000000000, 0.000000000000000000, 1.000000000000000000 ) ) ;
#21325 = CARTESIAN_POINT ( 'NONE',  ( -20.18153419852512442, 14.25141268122526483, -233.5059133483111964 ) ) ;
#21326 = CARTESIAN_POINT ( 'NONE',  ( -15.00242079508237936, 7.335218745534954898, -232.9526071471669013 ) ) ;
#21327 = CARTESIAN_POINT ( 'NONE',  ( 4.238595127209166868, 26.19205419861516404, -230.1142052665570077 ) ) ;
#21328 = DIRECTION ( 'NONE',  ( -2.891205793294678696E-17, 0.000000000000000000, -1.000000000000000000 ) ) ;
#21329 = CARTESIAN_POINT ( 'NONE',  ( 28.46362550855882745, 7.392895870364313282, -223.4682258299149566 ) ) ;
#21330 = CARTESIAN_POINT ( 'NONE',  ( -8.696851061449722309, -24.60219662023354914, -220.1357990587600852 ) ) ;
#21331 = ORIENTED_EDGE ( 'NONE', *, *, #20117, .T. ) ;
#21332 = CARTESIAN_POINT ( 'NONE',  ( 16.64575860537911112, 25.12688477742292648, -227.5050599151411745 ) ) ;
#21333 = CARTESIAN_POINT ( 'NONE',  ( -12.14452111807825041, 26.21581784948545035, -221.1455569020914140 ) ) ;
#21334 = CARTESIAN_POINT ( 'NONE',  ( -11.83206531956964902, 10.60028422373495260, -231.1115289952381033 ) ) ;
#21335 = CARTESIAN_POINT ( 'NONE',  ( -26.50758677328550306, -10.71756779952945671, -226.4207925882492987 ) ) ;
#21336 = CARTESIAN_POINT ( 'NONE',  ( -3.000000000000033751, 0.000000000000000000, -227.9999999999999716 ) ) ;
#21337 = VERTEX_POINT ( 'NONE', #2837 ) ;
#21338 = CARTESIAN_POINT ( 'NONE',  ( -24.48580119005125866, 9.312492396273500006, -232.5498413856076070 ) ) ;
#21339 = CARTESIAN_POINT ( 'NONE',  ( -9.935407011182972425, -19.19496561732008999, -215.7587022423821850 ) ) ;
#21340 = CARTESIAN_POINT ( 'NONE',  ( 15.04627082534134175, 1.516717341649120865, -227.5893993471154317 ) ) ;
#21341 = CIRCLE ( 'NONE', #2295, 16.23205080756887853 ) ;
#21342 = CARTESIAN_POINT ( 'NONE',  ( -6.474151797443945533, 21.29193859232740138, -215.9573456447696458 ) ) ;
#21343 = CARTESIAN_POINT ( 'NONE',  ( 14.75092884331204957, -2.920601562751602209, -225.7127978773227426 ) ) ;
#21344 = UNCERTAINTY_MEASURE_WITH_UNIT (LENGTH_MEASURE( 1.000000000000000082E-05 ), #11346, 'distance_accuracy_value', 'NONE');
#21345 = CARTESIAN_POINT ( 'NONE',  ( -15.94549496081242346, -0.04271059606100771622, -224.7066567765017169 ) ) ;
#21346 = CARTESIAN_POINT ( 'NONE',  ( 18.39533937270110187, 14.26564464607222504, -233.9088367426310242 ) ) ;
#21347 = CARTESIAN_POINT ( 'NONE',  ( 25.33562512631297281, 12.25422971834577268, -228.6777356031426791 ) ) ;
#21348 = FACE_OUTER_BOUND ( 'NONE', #19296, .T. ) ;
#21349 = CARTESIAN_POINT ( 'NONE',  ( -22.35595593184171292, -2.191382721379458332, -235.3044553127160441 ) ) ;
#21351 = EDGE_CURVE ( 'NONE', #11981, #17126, #10266, .T. ) ;
#21350 = CARTESIAN_POINT ( 'NONE',  ( -8.878187501988019648, -11.23476449186280846, -221.0271673637577123 ) ) ;
#21352 = CARTESIAN_POINT ( 'NONE',  ( 1.292981098121811279, -26.53499626907933262, -232.9055005154886828 ) ) ;
#21353 =( REPRESENTATION_RELATIONSHIP ('NONE','NONE', #5277, #14642 ) REPRESENTATION_RELATIONSHIP_WITH_TRANSFORMATION ( #4430 )SHAPE_REPRESENTATION_RELATIONSHIP( ) );
#21354 = DIRECTION ( 'NONE',  ( -1.000000000000000000, 0.000000000000000000, 0.000000000000000000 ) ) ;
#21355 = AXIS2_PLACEMENT_3D ( 'NONE', #15374, #13678, #17056 ) ;
#21356 = LINE ( 'NONE', #2457, #9820 ) ;
#21357 = CARTESIAN_POINT ( 'NONE',  ( -6.702936938788568888, 25.88675107068059944, -218.1129661040884287 ) ) ;
#21358 = CARTESIAN_POINT ( 'NONE',  ( 11.13603681652449318, -5.602932040673746172, -228.8141337797931101 ) ) ;
#21359 = CARTESIAN_POINT ( 'NONE',  ( 15.05686526350529775, -5.555778903407086133, -220.1433349335996468 ) ) ;
#21360 = CARTESIAN_POINT ( 'NONE',  ( -15.30864812529618391, 1.596444765892653717, -220.3859421844601627 ) ) ;
#21361 = CARTESIAN_POINT ( 'NONE',  ( 17.31940731551425827, 24.90170669671083914, -222.9868986272316533 ) ) ;
#21362 = CARTESIAN_POINT ( 'NONE',  ( 9.132190541728901323, 17.73033835127231939, -219.5524510795130766 ) ) ;
#21363 = ORIENTED_EDGE ( 'NONE', *, *, #6828, .T. ) ;
#21364 = CARTESIAN_POINT ( 'NONE',  ( 5.681636183907174065, -27.87860296351749767, -230.4665658140699804 ) ) ;
#21365 = DIRECTION ( 'NONE',  ( -1.000000000000000000, 0.000000000000000000, 0.000000000000000000 ) ) ;
#21366 = CARTESIAN_POINT ( 'NONE',  ( -12.80532875684362715, 24.61139456694233374, -232.5885756414849084 ) ) ;
#21367 = CARTESIAN_POINT ( 'NONE',  ( -19.61183938075907918, 22.25855138946451106, -229.5731876748794207 ) ) ;
#21368 = CARTESIAN_POINT ( 'NONE',  ( -23.08212926897555306, -14.71479305961103101, -218.7697472404056214 ) ) ;
#21369 = EDGE_CURVE ( 'NONE', #2436, #20426, #18537, .T. ) ;
#21370 = CARTESIAN_POINT ( 'NONE',  ( -23.52999999174766543, 19.39566142560855866, -221.9446938626390704 ) ) ;
#21371 = EDGE_CURVE ( 'NONE', #13588, #8719, #9611, .T. ) ;
#21372 = CARTESIAN_POINT ( 'NONE',  ( 17.01060404384151781, -6.151862203644831162, -218.3248062500343849 ) ) ;
#21373 = EDGE_CURVE ( 'NONE', #3236, #1365, #20309, .T. ) ;
#21374 = CARTESIAN_POINT ( 'NONE',  ( -5.762781846020777365, 12.94769902409342777, -223.1319556069387886 ) ) ;
#21375 = STYLED_ITEM ( 'NONE', ( #9765 ), #20907 ) ;
#21376 = CARTESIAN_POINT ( 'NONE',  ( 12.71499452845021416, 2.172589307656224378, -223.9381607050773084 ) ) ;
#21377 = CARTESIAN_POINT ( 'NONE',  ( -9.749377714296398878, 10.28442384816749922, -229.3722863967025205 ) ) ;
#21378 = CARTESIAN_POINT ( 'NONE',  ( 20.23125423326388628, 7.836699765464857137, -217.8891354894872450 ) ) ;
#21379 = CARTESIAN_POINT ( 'NONE',  ( 0.000000000000000000, 23.00000000000000000, -55.00000000000000711 ) ) ;
#21380 = ORIENTED_EDGE ( 'NONE', *, *, #12149, .T. ) ;
#21381 = CARTESIAN_POINT ( 'NONE',  ( 5.079647427451626562, 16.77877517420371234, -220.7769382327915366 ) ) ;
#21382 = CARTESIAN_POINT ( 'NONE',  ( -15.58529874627549461, -6.917566422457355202, -219.0138643999995054 ) ) ;
#21383 = CARTESIAN_POINT ( 'NONE',  ( 11.87982377808925527, 10.85265283465803421, -229.5027252913499183 ) ) ;
#21384 = CARTESIAN_POINT ( 'NONE',  ( -9.206457440458645891, -21.52042488620018545, -217.0715276568171248 ) ) ;
#21385 = CARTESIAN_POINT ( 'NONE',  ( 21.13757381859901940, 0.8461838617116986816, -222.1166354392582889 ) ) ;
#21386 = CARTESIAN_POINT ( 'NONE',  ( -22.24722865165759345, 18.77558306771206986, -226.5077042908023941 ) ) ;
#21387 = CARTESIAN_POINT ( 'NONE',  ( 10.44758276073090109, -14.65753298717242714, -218.5965683461722904 ) ) ;
#21388 = CARTESIAN_POINT ( 'NONE',  ( 7.249842700832647147, 18.24319783868832801, -219.1110502051974720 ) ) ;
#21389 = CARTESIAN_POINT ( 'NONE',  ( -18.74633356284308761, 11.17209001323738704, -217.5809474206552068 ) ) ;
#21390 = CARTESIAN_POINT ( 'NONE',  ( -13.00859847561873117, 4.399982435993697649, -231.0885370824921097 ) ) ;
#21391 = CARTESIAN_POINT ( 'NONE',  ( -8.609577223708431148, -18.69066821291321290, -217.1995118692595099 ) ) ;
#21392 = CIRCLE ( 'NONE', #11704, 22.96914677622851642 ) ;
#21393 = CARTESIAN_POINT ( 'NONE',  ( 10.85325209735074559, 11.82487774067193342, -216.5214842375702062 ) ) ;
#21394 = DIRECTION ( 'NONE',  ( -4.408728476930457445E-15, 1.000000000000000000, 0.000000000000000000 ) ) ;
#21395 = CARTESIAN_POINT ( 'NONE',  ( -19.75796449794633602, -18.82837501718038453, -216.0857152239166794 ) ) ;
#21396 = CARTESIAN_POINT ( 'NONE',  ( 3.367418898937407867, 27.20023797116225595, -219.3349021808245709 ) ) ;
#21397 = CARTESIAN_POINT ( 'NONE',  ( 26.28575214971901630, 3.591103948354015696, -217.0994821834097763 ) ) ;
#21398 = CARTESIAN_POINT ( 'NONE',  ( -5.762781846020777365, 12.94769902409342777, -223.1319556069387886 ) ) ;
#21399 = CARTESIAN_POINT ( 'NONE',  ( 15.23494377589453919, 15.24947835004434538, -215.7641128510430519 ) ) ;
#21400 = AXIS2_PLACEMENT_3D ( 'NONE', #478, #19147, #3726 ) ;
#21401 = CARTESIAN_POINT ( 'NONE',  ( 1.866975752136456279, -28.95217164724439840, -224.5474425503401221 ) ) ;
#21402 = PRESENTATION_LAYER_ASSIGNMENT (  '', '', ( #4162 ) ) ;
#21403 = CARTESIAN_POINT ( 'NONE',  ( -7.182761810198031505, -27.78193072152378207, -222.3754761716870973 ) ) ;
#21404 = EDGE_CURVE ( 'NONE', #18247, #13588, #11407, .T. ) ;
#21405 = CARTESIAN_POINT ( 'NONE',  ( 25.18785298611088308, 3.974282393449815931, -218.7636041058819956 ) ) ;
#21406 = CARTESIAN_POINT ( 'NONE',  ( 13.91151814069282722, -15.58123622716646572, -216.5183035683795367 ) ) ;
#21407 = CARTESIAN_POINT ( 'NONE',  ( -19.31342342724724759, -3.870051895940637365, -217.8584481481169348 ) ) ;
#21408 = CARTESIAN_POINT ( 'NONE',  ( -15.74157322273402748, -13.22745315869835636, -216.7831660370879661 ) ) ;
#21409 = CARTESIAN_POINT ( 'NONE',  ( 14.61121792518381390, 23.81825453963186590, -227.9329146581663110 ) ) ;
#21410 = CARTESIAN_POINT ( 'NONE',  ( 0.000000000000000000, 0.000000000000000000, 95.00000000000000000 ) ) ;
#21411 = CARTESIAN_POINT ( 'NONE',  ( -21.07387565400155438, 1.107905485989369554, -215.0000000023499069 ) ) ;
#21412 = CARTESIAN_POINT ( 'NONE',  ( 0.6364901924797052857, 13.89978473517355617, -221.8840706290426397 ) ) ;
#21413 = CARTESIAN_POINT ( 'NONE',  ( -0.3589900283600636066, 18.35437183075527656, -220.3960288481451357 ) ) ;
#21414 = CARTESIAN_POINT ( 'NONE',  ( 28.08871713846552254, -6.057249427443905709, -231.1189077393881348 ) ) ;
#21415 = EDGE_LOOP ( 'NONE', ( #7499, #10257, #7746, #8776, #14610, #16981 ) ) ;
#21416 = CARTESIAN_POINT ( 'NONE',  ( 13.82984244654956107, 22.51831320572884820, -232.1830460045772213 ) ) ;
#21417 = CARTESIAN_POINT ( 'NONE',  ( -12.01777041390050726, 10.97692933293401474, -227.6853890888168053 ) ) ;
#21418 = CARTESIAN_POINT ( 'NONE',  ( -16.75232826114664775, 4.232868982398014346, -229.4158550594996200 ) ) ;
#21419 = CARTESIAN_POINT ( 'NONE',  ( 6.250374750423979719, -27.98416211894771521, -222.2453514702945085 ) ) ;
#21421 = DIRECTION ( 'NONE',  ( 0.000000000000000000, 0.000000000000000000, -1.000000000000000000 ) ) ;
#21420 = AXIS2_PLACEMENT_3D ( 'NONE', #4122, #10675, #11003 ) ;
#21422 = EDGE_LOOP ( 'NONE', ( #516, #15601, #11833, #15007 ) ) ;
#21423 = CARTESIAN_POINT ( 'NONE',  ( 2.539761864897490007, 23.64215977235053501, -233.4645566207487661 ) ) ;
#21424 = CARTESIAN_POINT ( 'NONE',  ( 19.27468327664662695, -19.23223527390535637, -221.0469535581208618 ) ) ;
#21425 = CARTESIAN_POINT ( 'NONE',  ( -27.52457542293397097, 5.447957517019466067, -230.2717933641555135 ) ) ;
#21426 = CARTESIAN_POINT ( 'NONE',  ( -13.13432812001650341, -19.42279346457301514, -216.4126494286626610 ) ) ;
#21427 = APPLICATION_PROTOCOL_DEFINITION ( 'draft international standard', 'automotive_design', 1998, #14059 ) ;
#21428 = CARTESIAN_POINT ( 'NONE',  ( 4.603870848087811218, 30.13529352683433515, -225.9623629403671430 ) ) ;
#21429 = CARTESIAN_POINT ( 'NONE',  ( -2.218529449563984901, 24.06491599887877442, -214.8915873797660652 ) ) ;
#21430 = ORIENTED_EDGE ( 'NONE', *, *, #19039, .F. ) ;
#21431 = CARTESIAN_POINT ( 'NONE',  ( -23.52999999174766543, 19.39566142560855866, -221.9446938626390704 ) ) ;
#21432 = CARTESIAN_POINT ( 'NONE',  ( -22.73457989858237127, -6.881456255901889030, -216.4806380023168799 ) ) ;
#21433 = CYLINDRICAL_SURFACE ( 'NONE', #108, 17.50000000000007816 ) ;
#21434 = FACE_OUTER_BOUND ( 'NONE', #20589, .T. ) ;
#21435 = CARTESIAN_POINT ( 'NONE',  ( -18.39892766464214446, 25.11039525536027739, -225.3444503920457294 ) ) ;
#21436 = CARTESIAN_POINT ( 'NONE',  ( -11.08668407991722304, -24.47826551258279082, -233.9784602105897875 ) ) ;
#21437 = CARTESIAN_POINT ( 'NONE',  ( 13.38839277810360429, -5.174145297632733786, -223.8523798909600941 ) ) ;
#21438 = CARTESIAN_POINT ( 'NONE',  ( -17.17400284685640344, 24.63223427531467280, -220.6313524368512162 ) ) ;
#21439 = CARTESIAN_POINT ( 'NONE',  ( -27.12694304224540076, 7.756125161462346540, -217.3817363082233101 ) ) ;
#21440 = CARTESIAN_POINT ( 'NONE',  ( -1.248802714212398968, 14.93471382136348602, -228.4293827518713158 ) ) ;
#21441 = CARTESIAN_POINT ( 'NONE',  ( -14.10849459794400751, -0.2436790717799666162, -223.1085195285415921 ) ) ;
#21442 = CARTESIAN_POINT ( 'NONE',  ( -13.63442241228529994, 1.608023091903783008, -219.2326980015357094 ) ) ;
#21443 = CARTESIAN_POINT ( 'NONE',  ( -11.27700245477877772, -16.92453807419676792, -219.4498264308321609 ) ) ;
#21444 = ORIENTED_EDGE ( 'NONE', *, *, #12643, .F. ) ;
#21445 = EDGE_CURVE ( 'NONE', #215, #11287, #13508, .T. ) ;
#21446 = CARTESIAN_POINT ( 'NONE',  ( 7.163080459435270164, 24.05253566895842354, -232.4475987112033408 ) ) ;
#21447 = CARTESIAN_POINT ( 'NONE',  ( -15.77374768176864173, 20.07639682234129097, -218.6858893794192795 ) ) ;
#21448 = CARTESIAN_POINT ( 'NONE',  ( -10.76972226383489506, 9.682563335906554158, -229.2555443445334333 ) ) ;
#21449 = CARTESIAN_POINT ( 'NONE',  ( -21.98560163549725033, -7.841739570055646702, -218.0982455035688474 ) ) ;
#21450 = CARTESIAN_POINT ( 'NONE',  ( -25.00000000000013500, 1.972152263052529514E-28, 0.000000000000000000 ) ) ;
#21451 = ORIENTED_EDGE ( 'NONE', *, *, #9228, .T. ) ;
#21452 = CARTESIAN_POINT ( 'NONE',  ( -13.10651848559790444, 3.262242204071156948, -224.3513854875720597 ) ) ;
#21453 = CARTESIAN_POINT ( 'NONE',  ( -9.899145469884247817, -15.57979392722981693, -233.4163339629578786 ) ) ;
#21454 = CARTESIAN_POINT ( 'NONE',  ( 13.55929460187270053, 0.3562519042583365270, -227.9787723277739246 ) ) ;
#21455 = CARTESIAN_POINT ( 'NONE',  ( -3.843007962268670585, 27.94983497691806917, -231.4302614368887703 ) ) ;
#21456 = CARTESIAN_POINT ( 'NONE',  ( 14.85732601811957032, -2.750407783650710591, -223.7864485853946519 ) ) ;
#21457 = CARTESIAN_POINT ( 'NONE',  ( -18.94444594796027914, 3.458349568010113728, -218.9807021659310635 ) ) ;
#21458 = CARTESIAN_POINT ( 'NONE',  ( 19.20222574149634909, 21.83532798770326266, -218.6913543321078919 ) ) ;
#21459 = CARTESIAN_POINT ( 'NONE',  ( 21.53262694368047647, 11.06794636811408594, -231.8394491640143826 ) ) ;
#21460 = DIRECTION ( 'NONE',  ( -0.000000000000000000, -0.000000000000000000, -1.000000000000000000 ) ) ;
#21461 = CARTESIAN_POINT ( 'NONE',  ( -21.73784594492672895, -5.247588939251936146, -214.6321000900504714 ) ) ;
#21462 = CARTESIAN_POINT ( 'NONE',  ( -28.30937415889876618, -7.921132361018833556, -222.9755670691803857 ) ) ;
#21463 = CARTESIAN_POINT ( 'NONE',  ( 0.000000000000000000, -23.00000000000006040, -75.00000000000000000 ) ) ;
#21464 = CARTESIAN_POINT ( 'NONE',  ( 0.000000000000000000, 0.000000000000000000, -100.7764571353075524 ) ) ;
#21465 = CARTESIAN_POINT ( 'NONE',  ( -1.243734262319729389, 14.23902626181890518, -226.4313640849764795 ) ) ;
#21466 = CARTESIAN_POINT ( 'NONE',  ( 31.97344890504648518, -0.7122400102224841767, -225.1892660388073466 ) ) ;
#21467 = CARTESIAN_POINT ( 'NONE',  ( 16.85953475301105442, -7.801609028127129086, -231.9437213283852941 ) ) ;
#21468 = CARTESIAN_POINT ( 'NONE',  ( -21.43408368508570305, 3.680162304907783621, -233.1134812316964542 ) ) ;
#21469 = CARTESIAN_POINT ( 'NONE',  ( 11.43247012502872728, 12.44034019618676190, -231.9336559008378629 ) ) ;
#21470 = CARTESIAN_POINT ( 'NONE',  ( 12.84032013659066251, 19.10303921738740485, -230.8110334357214128 ) ) ;
#21471 = VERTEX_POINT ( 'NONE', #13887 ) ;
#21472 = CARTESIAN_POINT ( 'NONE',  ( 5.319567441806261066, -29.83260615907786573, -224.9444841741296841 ) ) ;
#21473 = CARTESIAN_POINT ( 'NONE',  ( 10.85304084868705843, 9.631209652036005764, 93.00000000000002842 ) ) ;
#21474 = CARTESIAN_POINT ( 'NONE',  ( 4.849508625227819003, 24.02665844953846275, -214.9607406399067315 ) ) ;
#21475 = CARTESIAN_POINT ( 'NONE',  ( -5.582510911615395699, 27.25430150734737111, -233.3200100877314469 ) ) ;
#21476 = CARTESIAN_POINT ( 'NONE',  ( 22.35566739451469331, -4.954007294914331894, -217.4158986454943374 ) ) ;
#21477 = CARTESIAN_POINT ( 'NONE',  ( -3.368164009525018265, 19.03203264544105622, -233.5986411977714567 ) ) ;
#21478 = CARTESIAN_POINT ( 'NONE',  ( -8.814245471595155479, -11.67815946035151775, 92.99999999999997158 ) ) ;
#21479 = ADVANCED_FACE ( 'NONE', ( #145 ), #15565, .T. ) ;
#21480 = CARTESIAN_POINT ( 'NONE',  ( -6.255852670334142829, 13.96671599789818252, -220.4426911866496823 ) ) ;
#21481 = CARTESIAN_POINT ( 'NONE',  ( 16.77642802340811556, -0.6192566135115280535, -218.8326447441449432 ) ) ;
#21482 = CARTESIAN_POINT ( 'NONE',  ( -9.171998067665157350, 9.395241133357435714, -226.3428046914542051 ) ) ;
#21483 = CARTESIAN_POINT ( 'NONE',  ( 22.46220731426537043, 18.23201731183003460, -227.5436199598787539 ) ) ;
#21484 = CARTESIAN_POINT ( 'NONE',  ( -23.30703516638871875, -0.6243632158918477337, -216.1214812734271220 ) ) ;
#21485 = EDGE_CURVE ( 'NONE', #15704, #21471, #13870, .T. ) ;
#21486 = ORIENTED_EDGE ( 'NONE', *, *, #17519, .F. ) ;
#21487 = CARTESIAN_POINT ( 'NONE',  ( -1.470815287892122125, 29.54293232078718745, -224.5855911371830302 ) ) ;
#21488 = CARTESIAN_POINT ( 'NONE',  ( -12.14186164972853810, -9.217338937739926408, -220.4665480714278374 ) ) ;
#21489 = CARTESIAN_POINT ( 'NONE',  ( 22.46220731426537043, 18.23201731183003460, -227.5436199598787539 ) ) ;
#21490 = CARTESIAN_POINT ( 'NONE',  ( 3.979505144402133876, -26.19079129315300491, -216.2323960841296469 ) ) ;
#21491 = DIRECTION ( 'NONE',  ( 1.224646799147353207E-16, 1.000000000000000000, 0.000000000000000000 ) ) ;
#21492 = CARTESIAN_POINT ( 'NONE',  ( -10.91003322996498071, 12.84665145358222382, -229.9786893781767958 ) ) ;
#21493 = DIRECTION ( 'NONE',  ( -2.891205793294678696E-17, 0.000000000000000000, -1.000000000000000000 ) ) ;
#21494 = CARTESIAN_POINT ( 'NONE',  ( 12.44471834243122466, -10.90083019301730083, -219.2211511521849161 ) ) ;
#21495 = CARTESIAN_POINT ( 'NONE',  ( 4.044213993247089967, 16.45246633354041421, -227.9255899743332918 ) ) ;
#21496 = CARTESIAN_POINT ( 'NONE',  ( -10.02095171162140019, 11.02119725306997111, -224.1251327387667516 ) ) ;
#21498 = AXIS2_PLACEMENT_3D ( 'NONE', #6940, #13810, #7391 ) ;
#21497 = CARTESIAN_POINT ( 'NONE',  ( -17.22166590524039265, 4.587137274468266135, -215.4863060638890033 ) ) ;
#21499 = CARTESIAN_POINT ( 'NONE',  ( -17.17062072939792117, -6.705141685950851027, -229.6398969478225354 ) ) ;
#21500 = CARTESIAN_POINT ( 'NONE',  ( 12.66989206167516357, 2.082990619159506007, -225.6419847029432901 ) ) ;
#21501 = DIRECTION ( 'NONE',  ( -0.000000000000000000, -0.000000000000000000, -1.000000000000000000 ) ) ;
#21502 = CARTESIAN_POINT ( 'NONE',  ( -24.71505016400469756, -15.67489082254766508, -232.1683526798342143 ) ) ;
#21503 = CARTESIAN_POINT ( 'NONE',  ( -4.866400999161825780, 25.69921167300892861, -231.0100031340613782 ) ) ;
#21504 = CARTESIAN_POINT ( 'NONE',  ( 21.96352831578506937, -0.3315607655626218175, -233.9427286327412787 ) ) ;
#21505 = SHAPE_REPRESENTATION ( 'motor', ( #6677 ), #1652 ) ;
#21506 = CARTESIAN_POINT ( 'NONE',  ( -6.581016643627174645, 27.50493254600863935, -230.8763182197739070 ) ) ;
#21507 = CARTESIAN_POINT ( 'NONE',  ( 4.719925043692215993, 22.16918918211828782, -214.6883144083888908 ) ) ;
#21508 = CARTESIAN_POINT ( 'NONE',  ( 8.467778565514151978, -25.57602835425881338, -228.7153423394380525 ) ) ;
#21509 = ORIENTED_EDGE ( 'NONE', *, *, #17580, .F. ) ;
#21510 = CARTESIAN_POINT ( 'NONE',  ( -1.544051355262263225, -15.46116467022245011, -222.0171457641791903 ) ) ;
#21511 = CARTESIAN_POINT ( 'NONE',  ( 26.48990917286906921, 12.16675355942207659, -225.0153622588060216 ) ) ;
#21512 = CARTESIAN_POINT ( 'NONE',  ( 9.918856707546316542, -11.48950767347732871, -219.9734948840342668 ) ) ;
#21513 = CARTESIAN_POINT ( 'NONE',  ( -26.07210576407111446, -8.413030596423759278, -230.6002792590230115 ) ) ;
#21514 = CARTESIAN_POINT ( 'NONE',  ( -9.625604265899946554, -19.21123364792547505, -233.9327940972253259 ) ) ;
#21515 = CARTESIAN_POINT ( 'NONE',  ( 6.136979247480394584, 21.37054498543370684, -230.9985475420231467 ) ) ;
#21516 = DIRECTION ( 'NONE',  ( -1.000000000000000000, 0.000000000000000000, 0.000000000000000000 ) ) ;
#21517 = CARTESIAN_POINT ( 'NONE',  ( -19.59898341672158040, 3.279988180491820504, -234.9371679595475086 ) ) ;
#21518 = CARTESIAN_POINT ( 'NONE',  ( 9.586902571418640662, 24.43292817174309661, -231.9968623198229807 ) ) ;
#21519 = CARTESIAN_POINT ( 'NONE',  ( 9.214796078729456497, 26.59493510027307650, -225.5796848805584318 ) ) ;
#21520 = CARTESIAN_POINT ( 'NONE',  ( 16.95735638057670869, -14.83641200555466355, -235.2222363121530293 ) ) ;
#21521 = CARTESIAN_POINT ( 'NONE',  ( 7.018811797190238622, 13.93862807232938472, -230.2855929063610176 ) ) ;
#21522 = CARTESIAN_POINT ( 'NONE',  ( -19.33106196848021341, 9.919700385716687663, -219.0532654734256255 ) ) ;
#21523 = CARTESIAN_POINT ( 'NONE',  ( -16.48591407464216729, 7.092323989942422635, -218.8909951703408012 ) ) ;
#21524 = CARTESIAN_POINT ( 'NONE',  ( 1.304950495335150507, -16.28913491483048759, -229.3926418476436027 ) ) ;
#21525 = B_SPLINE_CURVE_WITH_KNOTS ( 'NONE', 3,
 ( #19442, #12492, #5270, #7096, #9002, #19339, #12597, #9230, #3585, #5378, #2015, #20911, #16090, #661, #21131, #1902, #15760, #5614 ),
 .UNSPECIFIED., .F., .F.,
 ( 4, 2, 2, 2, 2, 2, 2, 2, 4 ),
 ( 0.003300329909327527622, 0.003720080272119055328, 0.004139830634910583035, 0.004559580997702110741, 0.004979331360493638448, 0.005399081723285166154, 0.005818832086076694728, 0.006238582448868222434, 0.006658332811659750140 ),
 .UNSPECIFIED. ) ;
#21526 = DIRECTION ( 'NONE',  ( -1.000000000000000000, 0.000000000000000000, 0.000000000000000000 ) ) ;
#21527 = CARTESIAN_POINT ( 'NONE',  ( -23.00000000000000000, 0.000000000000000000, -69.99999999999998579 ) ) ;
#21528 = CARTESIAN_POINT ( 'NONE',  ( 14.95414693437772868, 8.262206471704862665, -230.1862972580043163 ) ) ;
#21529 = CARTESIAN_POINT ( 'NONE',  ( 21.42236089941604860, -11.78161700756472641, -230.3636358161748490 ) ) ;
#21530 = CYLINDRICAL_SURFACE ( 'NONE', #13694, 10.00000000000000000 ) ;
#21531 = CARTESIAN_POINT ( 'NONE',  ( -5.240862053303020573, -11.96147391800445270, -224.1453450823045443 ) ) ;
#21532 = PRODUCT_CONTEXT ( 'NONE', #19483, 'mechanical' ) ;
#21533 = CARTESIAN_POINT ( 'NONE',  ( 0.9908753270255351575, 13.79205759140780430, -228.0165926715089881 ) ) ;
#21534 = CARTESIAN_POINT ( 'NONE',  ( -4.365576370787875859, 13.02741211227440665, -230.2897948137907917 ) ) ;
#21535 = ORIENTED_EDGE ( 'NONE', *, *, #8137, .F. ) ;
#21536 = CARTESIAN_POINT ( 'NONE',  ( -18.39892766464214446, 25.11039525536027739, -225.3444503920457294 ) ) ;
#21537 = CARTESIAN_POINT ( 'NONE',  ( -27.10757994293576800, -10.52107906247675473, -229.7403242048749519 ) ) ;
#21538 = DIRECTION ( 'NONE',  ( 0.000000000000000000, 0.000000000000000000, -1.000000000000000000 ) ) ;
#21539 = CARTESIAN_POINT ( 'NONE',  ( -21.30892042260266095, 8.664836834455229564, -5.033828640834366652 ) ) ;
#21540 = EDGE_CURVE ( 'NONE', #17987, #3651, #14228, .T. ) ;
#21541 = CARTESIAN_POINT ( 'NONE',  ( -17.65835845419170624, 22.55329142274348442, -231.2673511165784532 ) ) ;
#21542 = CARTESIAN_POINT ( 'NONE',  ( -1.366762408920091598, -18.58806247050231875, -233.7525452272278699 ) ) ;
#21543 = CARTESIAN_POINT ( 'NONE',  ( 17.01060404384151781, -6.151862203644831162, -218.3248062500343849 ) ) ;
#21544 = CARTESIAN_POINT ( 'NONE',  ( -11.24282496690421596, 12.44430180464951086, -232.4405891940542404 ) ) ;
#21545 = CARTESIAN_POINT ( 'NONE',  ( 14.02802030611117878, 3.063901161068346646, -225.6350222114233475 ) ) ;
#21546 = ORIENTED_EDGE ( 'NONE', *, *, #15304, .T. ) ;
#21547 = CARTESIAN_POINT ( 'NONE',  ( -2.665457046508036942, 16.94988614842223029, -218.7621057649994896 ) ) ;
#21548 = DIRECTION ( 'NONE',  ( -1.000000000000000000, 0.000000000000000000, 0.000000000000000000 ) ) ;
#21549 = CARTESIAN_POINT ( 'NONE',  ( 23.74723497152361062, 5.524508269105988134, -217.6012181427065002 ) ) ;
#21550 = CARTESIAN_POINT ( 'NONE',  ( -18.48279503042009964, -19.02624011246567548, -221.2510238762918107 ) ) ;
#21551 = VERTEX_POINT ( 'NONE', #1612 ) ;
#21552 = CARTESIAN_POINT ( 'NONE',  ( -13.93825237094548619, 9.044872709574327985, -220.1275804576921757 ) ) ;
#21553 = CARTESIAN_POINT ( 'NONE',  ( 8.821742718405863215, 10.82866050966069160, -221.4785132813277642 ) ) ;
#21554 = CARTESIAN_POINT ( 'NONE',  ( 2.770531592831002143, 22.28948935999365943, -215.1307751200139649 ) ) ;
#21555 = VERTEX_POINT ( 'NONE', #6791 ) ;
#21556 = CARTESIAN_POINT ( 'NONE',  ( -15.65746202990257174, -5.535581341804817868, -220.4933418326074559 ) ) ;
#21557 = DIRECTION ( 'NONE',  ( 1.000000000000000000, 0.000000000000000000, 0.000000000000000000 ) ) ;
#21558 = ORIENTED_EDGE ( 'NONE', *, *, #17379, .F. ) ;
#21559 = CARTESIAN_POINT ( 'NONE',  ( -22.99617382825321599, 17.18101613848176967, -230.9512687019100099 ) ) ;
#21560 = CARTESIAN_POINT ( 'NONE',  ( -3.294080042861979862, -13.96442541267666826, -227.2909938985368683 ) ) ;
#21561 = CYLINDRICAL_SURFACE ( 'NONE', #8344, 23.00000000000000000 ) ;
#21562 = CARTESIAN_POINT ( 'NONE',  ( -3.326157069579807946, 13.92020081821418565, -220.5733722327383930 ) ) ;
#21563 = FACE_OUTER_BOUND ( 'NONE', #1293, .T. ) ;
#21564 = PRODUCT_DEFINITION_CONTEXT ( 'detailed design', #5686, 'design' ) ;
#21565 = CARTESIAN_POINT ( 'NONE',  ( -21.89065952084834166, -0.9940043559354216907, -218.9999999999999716 ) ) ;
#21566 = CARTESIAN_POINT ( 'NONE',  ( 11.41911493375616260, 8.796695304819765582, -229.7440655656592412 ) ) ;
#21567 = CARTESIAN_POINT ( 'NONE',  ( -23.51670878402428144, 8.485352115581564547, -5.301345601592732493 ) ) ;
#21568 = EDGE_CURVE ( 'NONE', #17859, #10528, #16808, .T. ) ;
#21569 = CLOSED_SHELL ( 'NONE', ( #16390, #3474, #6104, #11307, #18379, #19834, #2782, #10793, #6096, #5406, #10623, #7269, #746, #10494, #14589, #9551 ) ) ;
#21570 = CARTESIAN_POINT ( 'NONE',  ( 26.24002132888527328, 11.62331517472360964, -222.5300873157218859 ) ) ;
#21571 = CARTESIAN_POINT ( 'NONE',  ( 24.99999999999999645, 1.360023205165816762E-13, 0.000000000000000000 ) ) ;
#21572 = CARTESIAN_POINT ( 'NONE',  ( 15.00179858758994911, -7.185045179863253750, -227.1671253934038077 ) ) ;
#21573 = CARTESIAN_POINT ( 'NONE',  ( -16.05483997570105714, -7.226811045751038165, -218.5819178105544438 ) ) ;
#21574 = CARTESIAN_POINT ( 'NONE',  ( 0.000000000000000000, 0.000000000000000000, -25.00000000000000000 ) ) ;
#21575 = CARTESIAN_POINT ( 'NONE',  ( 0.000000000000000000, 0.000000000000000000, 75.00000000000000000 ) ) ;
#21576 = CARTESIAN_POINT ( 'NONE',  ( -1.386728072030569692, 16.52832439466973824, -230.7516952943509807 ) ) ;
#21577 = CARTESIAN_POINT ( 'NONE',  ( 10.56552815906878529, -5.142824638143381755, -223.3550139360156663 ) ) ;
#21578 = CARTESIAN_POINT ( 'NONE',  ( 13.38839277810360429, -5.174145297632733786, -223.8523798909600941 ) ) ;
#21579 = CARTESIAN_POINT ( 'NONE',  ( -21.19360951076126653, 12.15251088906093457, -217.9482185194656552 ) ) ;
#21580 = CARTESIAN_POINT ( 'NONE',  ( 13.10956039622986324, 4.581323766968698585, -221.0328522389722252 ) ) ;
#21581 = CARTESIAN_POINT ( 'NONE',  ( 11.05872493453861161, 12.09300746323778775, -226.7727269015348952 ) ) ;
#21582 = ORIENTED_EDGE ( 'NONE', *, *, #21099, .F. ) ;
#21583 = CARTESIAN_POINT ( 'NONE',  ( 11.73142668431994018, -22.53166313379442443, -233.8575593048731491 ) ) ;
#21584 = CARTESIAN_POINT ( 'NONE',  ( 0.000000000000000000, 0.000000000000000000, -77.51594804401857175 ) ) ;
#21585 = CARTESIAN_POINT ( 'NONE',  ( -12.14471622011552832, 3.716031503296523653, -220.6237729066402835 ) ) ;
#21586 = CARTESIAN_POINT ( 'NONE',  ( -4.877547524699579640, 12.94924496403020697, -219.3991240521417581 ) ) ;
#21587 = CARTESIAN_POINT ( 'NONE',  ( 4.569118550756183339, 31.72363458735121000, -222.3920438419263519 ) ) ;
#21588 = CARTESIAN_POINT ( 'NONE',  ( 15.22026983281163481, -5.531916908390004828, -229.4891270354009123 ) ) ;
#21589 = CARTESIAN_POINT ( 'NONE',  ( -10.45786516112131892, 23.61456281964591852, -233.2869923610001592 ) ) ;
#21590 = CARTESIAN_POINT ( 'NONE',  ( -0.4310340159982842256, -14.49716617963122189, 93.00000000000000000 ) ) ;
#21591 = CARTESIAN_POINT ( 'NONE',  ( 2.471991688031208945, 13.88348721647344419, -230.6707754746932437 ) ) ;
#21592 = CARTESIAN_POINT ( 'NONE',  ( 22.49659352743751128, 7.060662713609715979, -215.7089950799439180 ) ) ;
#21593 = CARTESIAN_POINT ( 'NONE',  ( -27.90314475660494153, 12.48829126175061077, -223.3300566725355338 ) ) ;
#21594 = CARTESIAN_POINT ( 'NONE',  ( 13.03557269046774714, 7.519834803053426775, -226.9490612297269081 ) ) ;
#21595 = CARTESIAN_POINT ( 'NONE',  ( 6.729623925010410623, 16.84721552001897038, -219.9221131804260381 ) ) ;
#21596 = DIRECTION ( 'NONE',  ( 0.000000000000000000, 0.000000000000000000, -1.000000000000000000 ) ) ;
#21597 = CARTESIAN_POINT ( 'NONE',  ( 5.791579991237209235, 15.48299465423324861, -228.0203551130359472 ) ) ;
#21598 = CARTESIAN_POINT ( 'NONE',  ( -12.13177435108894642, -8.392035797555511323, -228.8392847287196332 ) ) ;
#21599 = CARTESIAN_POINT ( 'NONE',  ( 12.58590500897257947, 11.38573988265384607, -230.4867078522624695 ) ) ;
#21600 = CARTESIAN_POINT ( 'NONE',  ( -0.1762641309874839746, -13.43768854674724977, -229.3744256026976416 ) ) ;
#21601 = CARTESIAN_POINT ( 'NONE',  ( 19.25067847059919401, 2.577822808762952000, -223.4500418966247253 ) ) ;
#21602 = EDGE_CURVE ( 'NONE', #10678, #9167, #4494, .T. ) ;
#21603 = CARTESIAN_POINT ( 'NONE',  ( -10.40174557315337900, 22.75579539577861965, -231.4492192189165962 ) ) ;
#21604 = DIRECTION ( 'NONE',  ( 0.000000000000000000, 0.000000000000000000, -1.000000000000000000 ) ) ;
#21605 = CARTESIAN_POINT ( 'NONE',  ( 17.56598174185312899, -13.96259959359126768, -216.8519506175684626 ) ) ;
#21606 = CARTESIAN_POINT ( 'NONE',  ( 18.75523091462765990, 19.46592657336209697, -230.4909883316157391 ) ) ;
#21607 = CARTESIAN_POINT ( 'NONE',  ( -25.19248792833826300, 13.40115236862232528, -221.2817950683888455 ) ) ;
#21608 = CARTESIAN_POINT ( 'NONE',  ( -11.87391433320165746, 8.920676825367966245, -232.2044275666449096 ) ) ;
#21609 = CARTESIAN_POINT ( 'NONE',  ( -19.84632485794307399, -12.65249528142034485, -231.0223831579344278 ) ) ;
#21610 = CARTESIAN_POINT ( 'NONE',  ( 8.373295497769937867, 8.203271496719947820, -226.1884629658694053 ) ) ;
#21611 = AXIS2_PLACEMENT_3D ( 'NONE', #2632, #9513, #19837 ) ;
#21612 = DIRECTION ( 'NONE',  ( 0.000000000000000000, 0.000000000000000000, -1.000000000000000000 ) ) ;
#21613 = CARTESIAN_POINT ( 'NONE',  ( -9.442378551029269929, -6.949684989614740793, -225.4111852319283855 ) ) ;
#21614 = CARTESIAN_POINT ( 'NONE',  ( 2.464084843620814702, 29.35663482419208492, -227.0015060686748143 ) ) ;
#21615 = CARTESIAN_POINT ( 'NONE',  ( 12.25122766587143630, 4.035812653434439845, -225.7709573147497224 ) ) ;
#21616 = AXIS2_PLACEMENT_3D ( 'NONE', #13142, #11341, #11554 ) ;
#21617 = CARTESIAN_POINT ( 'NONE',  ( -12.33583941212908108, 22.27382123621224608, -231.6290720151527296 ) ) ;
#21618 = CARTESIAN_POINT ( 'NONE',  ( 9.100443535964535258, 24.01370002727352215, -234.5397711707082635 ) ) ;
#21619 = ORIENTED_EDGE ( 'NONE', *, *, #4856, .T. ) ;
#21620 = CARTESIAN_POINT ( 'NONE',  ( 7.754512012237808172, -26.66010948812077430, -222.3649102068104924 ) ) ;
#21621 = CARTESIAN_POINT ( 'NONE',  ( -7.086613078029399659, -28.17108726511417771, -223.6412629831645233 ) ) ;
#21622 = VECTOR ( 'NONE', #9353, 1000.000000000000000 ) ;
#21623 = CARTESIAN_POINT ( 'NONE',  ( -13.00859847561873117, 4.399982435993697649, -231.0885370824921097 ) ) ;
#21624 = CARTESIAN_POINT ( 'NONE',  ( 25.83609367470520723, -15.13481494965009411, -225.4685613576401124 ) ) ;
#21625 = CARTESIAN_POINT ( 'NONE',  ( -22.20848920810297855, -2.028924892417935055, -232.4401719831211039 ) ) ;
#21626 = CARTESIAN_POINT ( 'NONE',  ( -20.76924187596804217, -21.50248317380421170, -228.3679492147379335 ) ) ;
#21627 = CARTESIAN_POINT ( 'NONE',  ( 9.425340689562565544, 25.38932416188112384, -221.3391712389563963 ) ) ;
#21628 = DIRECTION ( 'NONE',  ( -1.000000000000000000, -6.982962677686272233E-15, 0.000000000000000000 ) ) ;
#21629 = CARTESIAN_POINT ( 'NONE',  ( 21.43345597994050777, 2.294722475943265838, -232.7243927205661294 ) ) ;
#21630 = CARTESIAN_POINT ( 'NONE',  ( 4.656903975822286768, 13.45000048768594780, -227.6722060245555497 ) ) ;
#21631 = CARTESIAN_POINT ( 'NONE',  ( -2.806347010929339802, 19.90767250424812573, -230.9206976900916004 ) ) ;
#21632 = CARTESIAN_POINT ( 'NONE',  ( 9.163585743560105357, -20.90777124155954425, -214.7369711139705259 ) ) ;
#21633 = CARTESIAN_POINT ( 'NONE',  ( 21.77183241683778547, 12.04504704525620085, -233.6005549158834640 ) ) ;
#21634 = CARTESIAN_POINT ( 'NONE',  ( -18.33565906012873725, 9.491905303418088025, -219.1855745749628568 ) ) ;
#21635 = CARTESIAN_POINT ( 'NONE',  ( -16.90857133559978465, -0.4126725064255206687, -221.6276144895144569 ) ) ;
#21636 = CARTESIAN_POINT ( 'NONE',  ( -6.454554286546707154, -27.99704349260872149, -227.4356265632874852 ) ) ;
#21637 = FACE_OUTER_BOUND ( 'NONE', #3264, .T. ) ;
#21638 = DIRECTION ( 'NONE',  ( -1.000000000000000000, 0.000000000000000000, 0.000000000000000000 ) ) ;
#21639 = VECTOR ( 'NONE', #21135, 1000.000000000000000 ) ;
#21640 = CARTESIAN_POINT ( 'NONE',  ( 10.55627441269396094, 10.31758739525044888, -223.1990319438957613 ) ) ;
#21641 = CARTESIAN_POINT ( 'NONE',  ( 23.95414175253014477, -14.38191447464009087, -225.3623377062671125 ) ) ;
#21642 = CARTESIAN_POINT ( 'NONE',  ( -29.22672729369577738, 6.588740615114764054, -224.9915299386302934 ) ) ;
#21643 = EDGE_CURVE ( 'NONE', #7031, #4726, #8259, .T. ) ;
#21644 = CARTESIAN_POINT ( 'NONE',  ( -12.42894476027428929, -17.97759322220185396, -216.3110355466728834 ) ) ;
#21645 =( NAMED_UNIT ( * ) PLANE_ANGLE_UNIT ( ) SI_UNIT ( $, .RADIAN. ) );
#21646 = EDGE_CURVE ( 'NONE', #10628, #2661, #14947, .T. ) ;
#21647 = CARTESIAN_POINT ( 'NONE',  ( -3.060450601941519189, 13.29454208326677289, -222.0135664617158682 ) ) ;
#21648 = CARTESIAN_POINT ( 'NONE',  ( -4.678665819194652187, 12.50541869316310262, -220.1509054161798247 ) ) ;
#21649 = VERTEX_POINT ( 'NONE', #1724 ) ;
#21650 = CARTESIAN_POINT ( 'NONE',  ( -4.620781219515533778, 16.99182040716223696, -217.1278208835672672 ) ) ;
#21651 = CARTESIAN_POINT ( 'NONE',  ( -30.78084016402396372, -2.501288241119758116, -224.5721874330603214 ) ) ;
#21652 = CARTESIAN_POINT ( 'NONE',  ( -23.05250587634771620, -9.674800950679635747, 2.613507269777442410 ) ) ;
#21653 = CARTESIAN_POINT ( 'NONE',  ( 17.50000000000001066, 0.000000000000000000, -30.00000000000000000 ) ) ;
#21654 = CARTESIAN_POINT ( 'NONE',  ( -4.620781219515533778, 16.99182040716223696, -217.1278208835672672 ) ) ;
#21655 = MANIFOLD_SOLID_BREP ( 'Mirror2', #6121 ) ;
#21656 = CARTESIAN_POINT ( 'NONE',  ( -4.737391463177558215, -17.33199396152823368, -215.7912354007318925 ) ) ;
#21657 = AXIS2_PLACEMENT_3D ( 'NONE', #1368, #4732, #12860 ) ;
#21658 = CARTESIAN_POINT ( 'NONE',  ( 25.46470895113276711, -14.41152162994631070, -228.1811935238409035 ) ) ;
#21659 = CARTESIAN_POINT ( 'NONE',  ( -6.474151797443945533, 21.29193859232740138, -215.9573456447696458 ) ) ;
#21660 = AXIS2_PLACEMENT_3D ( 'NONE', #12656, #5564, #7267 ) ;
#21661 = CARTESIAN_POINT ( 'NONE',  ( -26.47501633019681577, 13.84484755257420119, -230.0154374881822719 ) ) ;
#21662 = CARTESIAN_POINT ( 'NONE',  ( 0.7903203334012884884, 21.30772501796948859, -217.9064416298261619 ) ) ;
#21663 = CARTESIAN_POINT ( 'NONE',  ( -14.29986196492902550, 0.06805469746732484282, -227.4167624117703213 ) ) ;
#21664 = CARTESIAN_POINT ( 'NONE',  ( 13.71585692689473213, 6.523039003617190801, -224.4540437369149402 ) ) ;
#21665 = CARTESIAN_POINT ( 'NONE',  ( -9.669661339602258820, -12.96780954771633532, -224.3029626631937106 ) ) ;
#21666 = VERTEX_POINT ( 'NONE', #13551 ) ;
#21667 = CARTESIAN_POINT ( 'NONE',  ( -9.954421844142357756, 11.21484508112568079, -226.0177122452137439 ) ) ;
#21668 = CARTESIAN_POINT ( 'NONE',  ( 16.69977105456987232, 16.51652889326612694, -233.6667933521891030 ) ) ;
#21669 = CARTESIAN_POINT ( 'NONE',  ( -0.1452471002967452851, 24.29564289358754081, -234.0861481044164805 ) ) ;
#21670 = CARTESIAN_POINT ( 'NONE',  ( -29.43130594997593974, -3.977420319584657360, -224.3854249914923571 ) ) ;
#21671 = CARTESIAN_POINT ( 'NONE',  ( -1.232595164407830946E-29, 17.50000000000007105, -55.00000000000000000 ) ) ;
#21672 = ORIENTED_EDGE ( 'NONE', *, *, #1440, .T. ) ;
#21673 = CARTESIAN_POINT ( 'NONE',  ( -10.30050448363967419, 10.07750059423401190, -220.1837019037183723 ) ) ;
#21674 = CARTESIAN_POINT ( 'NONE',  ( -13.06588638656279322, -26.69120070130052014, -220.2265807429280642 ) ) ;
#21675 = CARTESIAN_POINT ( 'NONE',  ( 10.85888002857596923, 15.81835858589122878, -232.3913150909872627 ) ) ;
#21676 = CARTESIAN_POINT ( 'NONE',  ( 0.000000000000000000, 21.63401512838747820, -77.51594804401857175 ) ) ;
#21677 = AXIS2_PLACEMENT_3D ( 'NONE', #20692, #4029, #3920 ) ;
#21678 = AXIS2_PLACEMENT_3D ( 'NONE', #13708, #20771, #8868 ) ;
#21679 = CARTESIAN_POINT ( 'NONE',  ( -23.43012680803641956, 15.46310457140252304, -230.0052977649806962 ) ) ;
#21680 = CARTESIAN_POINT ( 'NONE',  ( 8.343316395906509086, 11.57404413652245800, -231.1403332574589911 ) ) ;
#21681 =( NAMED_UNIT ( * ) PLANE_ANGLE_UNIT ( ) SI_UNIT ( $, .RADIAN. ) );
#21682 = DIRECTION ( 'NONE',  ( -0.000000000000000000, 0.000000000000000000, -1.000000000000000000 ) ) ;
#21683 = CARTESIAN_POINT ( 'NONE',  ( 21.25094435758043332, 17.68230636442804027, -229.7964888993842010 ) ) ;
#21684 = PLANE ( 'NONE',  #10927 ) ;
#21685 = CARTESIAN_POINT ( 'NONE',  ( -22.13988250630526267, 1.271659148212506141, -215.1660654604927458 ) ) ;
#21686 = CARTESIAN_POINT ( 'NONE',  ( -25.10035252441274167, -15.33546242866430198, -228.3913311683031964 ) ) ;
#21687 = CARTESIAN_POINT ( 'NONE',  ( -21.95785083786292802, -6.849083017255801487, -7.293401492409205211 ) ) ;
#21688 = FACE_OUTER_BOUND ( 'NONE', #11048, .T. ) ;
#21689 = CARTESIAN_POINT ( 'NONE',  ( -4.824452364631481416, 22.01523768541901305, -216.8350837474290245 ) ) ;
#21690 = CARTESIAN_POINT ( 'NONE',  ( 12.55122320111375700, -1.519965464208375749, -221.0350040576933281 ) ) ;
#21691 = CIRCLE ( 'NONE', #6972, 21.00000000000000000 ) ;
#21692 = CARTESIAN_POINT ( 'NONE',  ( 23.44296991241933981, -12.51566675729016964, -231.4065378011870564 ) ) ;
#21693 = CARTESIAN_POINT ( 'NONE',  ( -14.07336028695978314, 1.752429266630609828, -222.9750305084206161 ) ) ;
#21694 = CARTESIAN_POINT ( 'NONE',  ( 26.28575214971901630, 3.591103948354015696, -217.0994821834097763 ) ) ;
#21695 = CARTESIAN_POINT ( 'NONE',  ( 10.01015180241662605, 20.19019600914695900, -219.1042218506083543 ) ) ;
#21696 = AXIS2_PLACEMENT_3D ( 'NONE', #5915, #16170, #2316 ) ;
#21697 = CARTESIAN_POINT ( 'NONE',  ( -0.5904090961472509003, -15.19049578300894510, -228.4387523405810612 ) ) ;
#21698 = DIRECTION ( 'NONE',  ( 0.000000000000000000, 0.000000000000000000, -1.000000000000000000 ) ) ;
#21699 = CARTESIAN_POINT ( 'NONE',  ( -31.04415783139704388, 5.868882651865275690, -221.1472518903637194 ) ) ;
#21700 = CARTESIAN_POINT ( 'NONE',  ( 7.174260007897984792, 9.971262771497068300, -226.2872513832048469 ) ) ;
#21701 = CARTESIAN_POINT ( 'NONE',  ( 4.849508625227819003, 24.02665844953846275, -214.9607406399067315 ) ) ;
#21702 = CARTESIAN_POINT ( 'NONE',  ( 17.78250599636351481, -9.160802950715318360, -218.6762383290621869 ) ) ;
#21703 = CARTESIAN_POINT ( 'NONE',  ( 0.9046320824004248085, 13.39785254849979701, -226.4815711199935890 ) ) ;
#21704 = CARTESIAN_POINT ( 'NONE',  ( -13.69675006931110417, 3.702342960760605539, -228.0723273272095355 ) ) ;
#21705 = CARTESIAN_POINT ( 'NONE',  ( 11.31331191788792623, 29.23420701778062281, -220.7538464529627333 ) ) ;
#21706 = CARTESIAN_POINT ( 'NONE',  ( -25.11055959288653128, 8.701823109978603199, -230.2231080656787583 ) ) ;
#21707 = CARTESIAN_POINT ( 'NONE',  ( -19.00318367631585659, 13.14621133775862916, -233.8403879275295765 ) ) ;
#21708 = AXIS2_PLACEMENT_3D ( 'NONE', #5769, #21077, #17940 ) ;
#21709 = CARTESIAN_POINT ( 'NONE',  ( 28.02123297569005089, 5.903198806000402143, -227.5759114383273811 ) ) ;
#21710 = CARTESIAN_POINT ( 'NONE',  ( 3.635089269978064141, 27.05650967970794341, -222.4639105745756638 ) ) ;
#21711 = PLANE ( 'NONE',  #5473 ) ;
#21712 = CARTESIAN_POINT ( 'NONE',  ( 0.000000000000000000, 0.000000000000000000, 77.51594804401857175 ) ) ;
#21713 = CARTESIAN_POINT ( 'NONE',  ( 11.21155440434494643, 24.57152134148167733, -221.7155903571010356 ) ) ;
#21714 = CARTESIAN_POINT ( 'NONE',  ( -11.07688804854283049, -12.81333559660784971, -232.1241261852632363 ) ) ;
#21715 = CARTESIAN_POINT ( 'NONE',  ( 16.38151749656409351, 8.902090001712490874, -231.2955017965201989 ) ) ;
#21716 = CARTESIAN_POINT ( 'NONE',  ( -9.132447960227011663, -28.48575439045284696, -228.2342138548108892 ) ) ;
#21717 = DIRECTION ( 'NONE',  ( -0.000000000000000000, -0.000000000000000000, -1.000000000000000000 ) ) ;
#21718 = CARTESIAN_POINT ( 'NONE',  ( -4.742143146070755932, 15.01230778631049567, -221.4832709320255049 ) ) ;
#21719 = CARTESIAN_POINT ( 'NONE',  ( 10.62272209279942992, -9.818939940036045755, -222.1403336352628344 ) ) ;
#21720 = CARTESIAN_POINT ( 'NONE',  ( 25.40172858355122898, 15.07073195964820833, -229.0276483847865450 ) ) ;
#21721 = CARTESIAN_POINT ( 'NONE',  ( -7.250603130619442283, 20.89725557392719324, -217.7893896917081520 ) ) ;
#21722 = CARTESIAN_POINT ( 'NONE',  ( -21.85741505224184777, 1.741064654082184582, -235.1654459941842390 ) ) ;
#21723 = CARTESIAN_POINT ( 'NONE',  ( -18.47336874364275516, -4.831184938305232990, -219.8627234292127639 ) ) ;
#21724 = CARTESIAN_POINT ( 'NONE',  ( 14.17826651990317188, -1.167225063855702683, -222.4240311848849387 ) ) ;
#21725 = VECTOR ( 'NONE', #11710, 1000.000000000000000 ) ;
#21726 =( GEOMETRIC_REPRESENTATION_CONTEXT ( 3 ) GLOBAL_UNCERTAINTY_ASSIGNED_CONTEXT ( ( #875 ) ) GLOBAL_UNIT_ASSIGNED_CONTEXT ( ( #1097, #13032, #4802 ) ) REPRESENTATION_CONTEXT ( 'NONE', 'WORKASPACE' ) );
#21727 = PLANE ( 'NONE',  #15946 ) ;
#21728 = CARTESIAN_POINT ( 'NONE',  ( -30.46088052942827318, -8.161173215405806758, -225.9185547777119893 ) ) ;
#21729 = CARTESIAN_POINT ( 'NONE',  ( 21.26803326031697949, 19.54255073453192892, -230.5813148908474659 ) ) ;
#21730 = CARTESIAN_POINT ( 'NONE',  ( 24.81079154715000357, 3.171651085595392772, -216.4177249688571578 ) ) ;
#21731 = CARTESIAN_POINT ( 'NONE',  ( 3.001892273201697048, 27.20292285420111966, -216.7800154582108689 ) ) ;
#21732 = CARTESIAN_POINT ( 'NONE',  ( 7.587775680576782200, 20.81864918083767435, -235.2547171215352364 ) ) ;
#21733 = ORIENTED_EDGE ( 'NONE', *, *, #2519, .F. ) ;
#21734 = CARTESIAN_POINT ( 'NONE',  ( 4.834917880317126659, -18.50358955815650219, -219.1181532354089256 ) ) ;
#21735 = ORIENTED_EDGE ( 'NONE', *, *, #18546, .T. ) ;
#21736 = CARTESIAN_POINT ( 'NONE',  ( -7.180402128846711918, -26.42159752827261698, -220.2116303544826224 ) ) ;
#21737 = CARTESIAN_POINT ( 'NONE',  ( -12.61443312487471324, 8.399394471292156439, -217.5740162615319093 ) ) ;
#21738 = CARTESIAN_POINT ( 'NONE',  ( 9.104026917753444081, -10.66572815660443041, -221.9193219976906448 ) ) ;
#21739 = CARTESIAN_POINT ( 'NONE',  ( -16.20471097821853235, -2.781505378741172319, -220.1484675126197317 ) ) ;
#21740 = AXIS2_PLACEMENT_3D ( 'NONE', #447, #1905, #557 ) ;
#21741 = CARTESIAN_POINT ( 'NONE',  ( -11.28700884291539630, -21.85791790461604478, -233.5354093188319951 ) ) ;
#21742 = AXIS2_PLACEMENT_3D ( 'NONE', #2731, #6443, #9949 ) ;
#21743 = CARTESIAN_POINT ( 'NONE',  ( 11.83256327006771969, 5.988634687709346593, -225.8999299265561831 ) ) ;
#21744 = CARTESIAN_POINT ( 'NONE',  ( 0.000000000000000000, 0.000000000000000000, -70.00000000000000000 ) ) ;
#21745 = CARTESIAN_POINT ( 'NONE',  ( -11.07173923371951574, 9.938770595667456575, -229.9381419817434562 ) ) ;
#21746 = CARTESIAN_POINT ( 'NONE',  ( 19.61276001257277102, 19.97122404150989894, -229.5162757829903342 ) ) ;
#21747 = CARTESIAN_POINT ( 'NONE',  ( 11.13678936984666912, 26.95732789089726111, -228.8350761760834757 ) ) ;
#21748 = CARTESIAN_POINT ( 'NONE',  ( 16.97369223523349646, 15.19068754808448851, -217.0779026324121332 ) ) ;
#21749 = CARTESIAN_POINT ( 'NONE',  ( 7.391697205318404684, -9.868666992833734497, -221.1858763705714068 ) ) ;
#21750 = CARTESIAN_POINT ( 'NONE',  ( 25.38325563848796662, 11.05100313887457553, -217.8685524735130628 ) ) ;
#21751 = CARTESIAN_POINT ( 'NONE',  ( -9.679547659771646551, 14.60131434979866505, -230.4338124916943968 ) ) ;
#21752 = CARTESIAN_POINT ( 'NONE',  ( -13.01444359484612079, -23.32256785062423887, -219.1545357706015693 ) ) ;
#21753 = CARTESIAN_POINT ( 'NONE',  ( -20.94800339253696109, 4.477632454355491731, -216.5423208360950298 ) ) ;
#21754 = CARTESIAN_POINT ( 'NONE',  ( 0.000000000000000000, 0.000000000000000000, -24.99999999999999645 ) ) ;
#21755 = CARTESIAN_POINT ( 'NONE',  ( 24.57222455393806015, 12.08236629421828212, -229.7319216558644541 ) ) ;
#21756 = CARTESIAN_POINT ( 'NONE',  ( 23.31955656579280145, -13.39010844438576520, -228.3495985225334266 ) ) ;
#21757 = PLANE ( 'NONE',  #29 ) ;
#21758 = EDGE_CURVE ( 'NONE', #6969, #12003, #18719, .T. ) ;
#21759 = STYLED_ITEM ( 'NONE', ( #10724 ), #22038 ) ;
#21760 = CARTESIAN_POINT ( 'NONE',  ( -2.576162127940193169, -15.57202066281789321, -231.6911579627040396 ) ) ;
#21761 = CARTESIAN_POINT ( 'NONE',  ( -3.673551555920188783, 29.81207051619892923, -228.8770490300152005 ) ) ;
#21762 = CARTESIAN_POINT ( 'NONE',  ( -4.877547524699579640, 12.94924496403020697, -219.3991240521417581 ) ) ;
#21763 = ORIENTED_EDGE ( 'NONE', *, *, #17120, .F. ) ;
#21764 = CARTESIAN_POINT ( 'NONE',  ( 0.9908753270255351575, 13.79205759140780430, -228.0165926715089881 ) ) ;
#21765 = CARTESIAN_POINT ( 'NONE',  ( -16.30907414568449454, -3.310091733494833655, -231.8954501777161283 ) ) ;
#21766 = CARTESIAN_POINT ( 'NONE',  ( -24.04509347396444241, -6.847624739850214581, -7.294798726659911914 ) ) ;
#21767 = CARTESIAN_POINT ( 'NONE',  ( 0.000000000000000000, 22.63401512838748175, -77.51594804401857175 ) ) ;
#21768 = CARTESIAN_POINT ( 'NONE',  ( 5.248230734842167955, 23.54336384919183445, -216.8914391693808739 ) ) ;
#21769 = CARTESIAN_POINT ( 'NONE',  ( -13.66010072360327676, -23.28416639572314750, -215.9262288161416166 ) ) ;
#21770 = CARTESIAN_POINT ( 'NONE',  ( 15.65513449100897780, -26.00057195821942457, -227.4103383097017570 ) ) ;
#21771 = CARTESIAN_POINT ( 'NONE',  ( 15.54083024098960486, -10.44392130763852222, -217.6620978190037476 ) ) ;
#21772 = CARTESIAN_POINT ( 'NONE',  ( -12.33997807949817904, 15.01940705987184188, -217.6798968600957380 ) ) ;
#21773 = EDGE_CURVE ( 'NONE', #14565, #18158, #5580, .T. ) ;
#21774 = CARTESIAN_POINT ( 'NONE',  ( 8.312165662451315384, 13.84431584962456974, -225.8109542921768025 ) ) ;
#21775 = CARTESIAN_POINT ( 'NONE',  ( -26.02440924314744919, 2.824604386891162111, -232.0644005296583430 ) ) ;
#21776 = CARTESIAN_POINT ( 'NONE',  ( -21.12280458060320498, 13.61074013710079988, -216.5529903464332335 ) ) ;
#21777 = CARTESIAN_POINT ( 'NONE',  ( -25.45695634607983848, -10.72451519803311015, -228.5848280742264933 ) ) ;
#21778 = AXIS2_PLACEMENT_3D ( 'NONE', #14537, #18320, #18430 ) ;
#21779 = ORIENTED_EDGE ( 'NONE', *, *, #20690, .T. ) ;
#21780 = CARTESIAN_POINT ( 'NONE',  ( -17.99720854823001659, 13.97888873227035056, -232.2992184661552244 ) ) ;
#21781 = CARTESIAN_POINT ( 'NONE',  ( 3.846342036506673612, 16.55327908958690131, -231.1358846258000597 ) ) ;
#21782 = CARTESIAN_POINT ( 'NONE',  ( -5.590964611773372894, 13.92546790642523113, -228.7941110425196882 ) ) ;
#21783 = CARTESIAN_POINT ( 'NONE',  ( -26.75342641616541783, -10.60804028525731546, -225.2137697103424898 ) ) ;
#21784 = CARTESIAN_POINT ( 'NONE',  ( 0.000000000000000000, 0.000000000000000000, -24.99999999999999645 ) ) ;
#21785 = ORIENTED_EDGE ( 'NONE', *, *, #586, .T. ) ;
#21786 = CARTESIAN_POINT ( 'NONE',  ( -15.58461825850822180, 18.91734573546571951, -233.7691177939990723 ) ) ;
#21787 = CARTESIAN_POINT ( 'NONE',  ( -2.916193397327769166, -13.79856165086501107, -222.9033574188488842 ) ) ;
#21788 = CARTESIAN_POINT ( 'NONE',  ( 14.73698509926073186, 4.443590625350892331, -227.4062002049096236 ) ) ;
#21789 = CARTESIAN_POINT ( 'NONE',  ( 17.68508104102419409, 23.41266195669770767, -227.5327139115408954 ) ) ;
#21790 = FACE_OUTER_BOUND ( 'NONE', #12588, .T. ) ;
#21791 = UNCERTAINTY_MEASURE_WITH_UNIT (LENGTH_MEASURE( 1.000000000000000082E-05 ), #11184, 'distance_accuracy_value', 'NONE');
#21792 = CARTESIAN_POINT ( 'NONE',  ( -22.91388766833460977, 0.000000000000000000, -75.05807060175870049 ) ) ;
#21793 = CARTESIAN_POINT ( 'NONE',  ( -14.30096418567650041, 6.974026439069829664, -228.7941652905285537 ) ) ;
#21794 = CARTESIAN_POINT ( 'NONE',  ( 17.89221702206198117, 0.2742047965568425449, -220.2420650470893122 ) ) ;
#21795 = SURFACE_STYLE_USAGE ( .BOTH. , #7970 ) ;
#21796 = CARTESIAN_POINT ( 'NONE',  ( -25.00000000000013500, 0.3339166901145541044, -10.00000000000000000 ) ) ;
#21797 = CARTESIAN_POINT ( 'NONE',  ( 18.76166303929371182, -3.000000000000011990, -224.8780544821428578 ) ) ;
#21798 = CARTESIAN_POINT ( 'NONE',  ( 0.000000000000000000, 0.000000000000000000, -99.99999999999998579 ) ) ;
#21799 = CARTESIAN_POINT ( 'NONE',  ( 17.22969587606878505, -8.834803756807117381, -230.2348533348707917 ) ) ;
#21800 = CARTESIAN_POINT ( 'NONE',  ( -25.98129645912436914, -15.13773040547512139, -224.1390156429105787 ) ) ;
#21801 = CARTESIAN_POINT ( 'NONE',  ( -22.38166440881320440, -5.304594382025126897, 8.483353619577671978 ) ) ;
#21802 = CARTESIAN_POINT ( 'NONE',  ( -24.63401512838747820, 0.000000000000000000, -77.51594804401857175 ) ) ;
#21803 = CARTESIAN_POINT ( 'NONE',  ( 5.248013545904832711, 18.51731616863089158, -219.3673127389703552 ) ) ;
#21804 = CARTESIAN_POINT ( 'NONE',  ( 18.59830189133340639, -20.05840858737748533, -233.4490516770458157 ) ) ;
#21805 = CARTESIAN_POINT ( 'NONE',  ( 28.52058947142581502, -1.755848367977142610, -221.9695116608532715 ) ) ;
#21806 = CARTESIAN_POINT ( 'NONE',  ( -17.39737143130126285, 7.531548707695031375, -232.0788227848755696 ) ) ;
#21807 = CARTESIAN_POINT ( 'NONE',  ( -15.83894155097017631, 1.950284868793920712, -224.5615909987450038 ) ) ;
#21808 = CARTESIAN_POINT ( 'NONE',  ( 13.38540196930496862, 9.639609424068478205, -227.8779021328794840 ) ) ;
#21809 = VERTEX_POINT ( 'NONE', #15126 ) ;
#21810 = CARTESIAN_POINT ( 'NONE',  ( 10.42186625103445152, -25.39807580958450473, -217.7675295214572202 ) ) ;
#21811 = CARTESIAN_POINT ( 'NONE',  ( 0.2467007162552592447, 14.49943138577569179, 93.00000000000001421 ) ) ;
#21812 = CARTESIAN_POINT ( 'NONE',  ( -30.66857674073067130, 4.440060741118782239, -229.9901150862898476 ) ) ;
#21813 = CARTESIAN_POINT ( 'NONE',  ( 3.764125772070460396, 11.78312483992801596, -228.3484643988637970 ) ) ;
#21814 = CARTESIAN_POINT ( 'NONE',  ( 4.754245974719506940, 31.05377813473586102, -220.6166503949300193 ) ) ;
#21815 = CARTESIAN_POINT ( 'NONE',  ( 13.86395146404758982, -8.823451364178625411, -228.3963352256065491 ) ) ;
#21816 = CARTESIAN_POINT ( 'NONE',  ( -3.755296588130283553, 23.77975947300719284, -233.7323173085780752 ) ) ;
#21817 = CARTESIAN_POINT ( 'NONE',  ( -27.90314475660494153, 12.48829126175061077, -223.3300566725355338 ) ) ;
#21818 = CARTESIAN_POINT ( 'NONE',  ( 13.32754126089433377, 12.31312334927721963, -234.6033665822900218 ) ) ;
#21819 = CARTESIAN_POINT ( 'NONE',  ( -15.54392142943450317, 6.670312097614393920, -219.6934017696036676 ) ) ;
#21820 = CARTESIAN_POINT ( 'NONE',  ( -2.698926868850080041, 12.89339462271858316, -226.7595176699009585 ) ) ;
#21821 = CARTESIAN_POINT ( 'NONE',  ( 22.02796522526679723, 16.41909032291435366, -220.1590600991317217 ) ) ;
#21822 = CARTESIAN_POINT ( 'NONE',  ( 14.61121792518381390, 23.81825453963186590, -227.9329146581663110 ) ) ;
#21823 = CARTESIAN_POINT ( 'NONE',  ( 23.36729170583618398, -5.500043712341283531, -232.1593072787115375 ) ) ;
#21824 = CARTESIAN_POINT ( 'NONE',  ( 0.000000000000000000, 0.000000000000000000, -120.0000000000000142 ) ) ;
#21825 = EDGE_CURVE ( 'NONE', #1266, #17843, #19249, .T. ) ;
#21826 = CARTESIAN_POINT ( 'NONE',  ( -14.93108815068229589, -1.792787290847115633, -227.6165763581034582 ) ) ;
#21827 = CARTESIAN_POINT ( 'NONE',  ( 10.78187269046063435, 10.73871010366167944, -221.9206544238666368 ) ) ;
#21828 = CARTESIAN_POINT ( 'NONE',  ( -9.447593206125553422, -28.82180577676834332, -226.7547558591687675 ) ) ;
#21829 = CARTESIAN_POINT ( 'NONE',  ( 18.93769218002320898, 2.849225658158390573, -225.9458950196911076 ) ) ;
#21830 = CARTESIAN_POINT ( 'NONE',  ( -11.03778527004271659, 26.96286968643956428, -225.4057095641571209 ) ) ;
#21831 = CARTESIAN_POINT ( 'NONE',  ( 13.66436340482409761, -13.84785698770488871, -232.6553000701566134 ) ) ;
#21832 = CARTESIAN_POINT ( 'NONE',  ( 16.43556216695724004, 8.397919695511960825, -216.7971521583719152 ) ) ;
#21833 = CARTESIAN_POINT ( 'NONE',  ( -8.317278876689359279, 23.15034512777772235, -218.2935523245793092 ) ) ;
#21834 = CARTESIAN_POINT ( 'NONE',  ( -5.861205904341304951, 14.21969934012253312, -219.3213214613830644 ) ) ;
#21835 = VERTEX_POINT ( 'NONE', #3399 ) ;
#21836 = CARTESIAN_POINT ( 'NONE',  ( -19.26019478805205054, -16.72235099301716943, -219.5158537523224993 ) ) ;
#21837 = CARTESIAN_POINT ( 'NONE',  ( 30.65249971456167799, 3.724008896938769464, -225.4815109119605552 ) ) ;
#21838 = CARTESIAN_POINT ( 'NONE',  ( -13.36635042947306573, -0.3940246778032021058, -227.3384152261055249 ) ) ;
#21839 = CARTESIAN_POINT ( 'NONE',  ( 18.81274554574540403, 10.85963742466947224, -234.0446454529665345 ) ) ;
#21840 = CARTESIAN_POINT ( 'NONE',  ( -21.26441444091935296, 10.69428164102106926, -219.3434466924981336 ) ) ;
#21841 = CARTESIAN_POINT ( 'NONE',  ( 1.220475224794998370, 29.83033731899746144, -230.4224274340063801 ) ) ;
#21842 = CARTESIAN_POINT ( 'NONE',  ( 8.343316395906509086, 11.57404413652245800, -231.1403332574589911 ) ) ;
#21843 = ORIENTED_EDGE ( 'NONE', *, *, #18896, .T. ) ;
#21844 = CARTESIAN_POINT ( 'NONE',  ( -16.91104737563547644, -22.20641354538343748, -232.3619262256263482 ) ) ;
#21845 = ADVANCED_FACE ( 'NONE', ( #8598 ), #12079, .T. ) ;
#21846 = ORIENTED_EDGE ( 'NONE', *, *, #7475, .F. ) ;
#21847 = CARTESIAN_POINT ( 'NONE',  ( 4.002939343642331949, -22.37368820207002429, -217.8631878264377804 ) ) ;
#21848 = CIRCLE ( 'NONE', #1737, 3.000000000000002665 ) ;
#21849 = CARTESIAN_POINT ( 'NONE',  ( -11.10150084103673684, 3.549415896002023896, -226.0408865487038952 ) ) ;
#21850 = CARTESIAN_POINT ( 'NONE',  ( 23.44296991241933981, -12.51566675729016964, -231.4065378011870564 ) ) ;
#21851 = CARTESIAN_POINT ( 'NONE',  ( -14.73155177304599306, -1.817590056890399763, -226.9769936995019748 ) ) ;
#21852 = CARTESIAN_POINT ( 'NONE',  ( -13.67406442719345883, -9.319000780081536206, -231.1492214949047934 ) ) ;
#21853 = CARTESIAN_POINT ( 'NONE',  ( 15.74259730902452858, 17.40808440793174583, -232.1327802909178786 ) ) ;
#21854 = CARTESIAN_POINT ( 'NONE',  ( 0.000000000000000000, 0.000000000000000000, -105.0000000000000142 ) ) ;
#21855 = CARTESIAN_POINT ( 'NONE',  ( -8.548213857283494477, 12.07277636836182211, -222.5354997492170241 ) ) ;
#21856 = CARTESIAN_POINT ( 'NONE',  ( 10.25308675723727347, 13.16459519580956972, -229.3963488176951273 ) ) ;
#21857 = CARTESIAN_POINT ( 'NONE',  ( -3.843007962268670585, 27.94983497691806917, -231.4302614368887703 ) ) ;
#21858 = CARTESIAN_POINT ( 'NONE',  ( 10.14297843322460402, 14.69845403004500639, -219.2805000163441207 ) ) ;
#21859 = CARTESIAN_POINT ( 'NONE',  ( 27.54866699188204748, -16.08959018098719085, -223.7550031907416326 ) ) ;
#21860 = CARTESIAN_POINT ( 'NONE',  ( -10.46043650402819125, 8.998596506756641134, -222.4402691847174083 ) ) ;
#21861 = CARTESIAN_POINT ( 'NONE',  ( -5.786930954831501772, 15.78543306641166311, -231.0475152612371517 ) ) ;
#21862 = CARTESIAN_POINT ( 'NONE',  ( -17.81508947870519322, -18.77243306401324219, -218.1930932538018340 ) ) ;
#21863 = DIRECTION ( 'NONE',  ( -1.000000000000000000, 0.000000000000000000, 0.000000000000000000 ) ) ;
#21864 = FACE_BOUND ( 'NONE', #17655, .T. ) ;
#21865 = CARTESIAN_POINT ( 'NONE',  ( 15.42212722119060864, 5.401662248084913465, -220.8333402320903645 ) ) ;
#21866 = CARTESIAN_POINT ( 'NONE',  ( 14.47405021949252557, -20.16114635186222159, -231.2055612633458566 ) ) ;
#21867 = CARTESIAN_POINT ( 'NONE',  ( -16.74094048923576494, 16.03040267675914521, -217.9177456399057178 ) ) ;
#21868 = AXIS2_PLACEMENT_3D ( 'NONE', #21450, #11012, #9325 ) ;
#21869 = CARTESIAN_POINT ( 'NONE',  ( 2.808299412262623473, 18.06245856371233316, -217.9832661743849656 ) ) ;
#21870 = CARTESIAN_POINT ( 'NONE',  ( -11.36971918743327237, -8.287084598727400220, -223.1364763414170227 ) ) ;
#21871 = ITEM_DEFINED_TRANSFORMATION ( 'NONE', 'NONE', #7080,  #6677 ) ;
#21872 = CARTESIAN_POINT ( 'NONE',  ( -24.48812334466693486, 4.469247780253509106, -230.3044243311433945 ) ) ;
#21873 = CARTESIAN_POINT ( 'NONE',  ( 14.02309809840729393, 19.05079204846204277, -234.6885355850075143 ) ) ;
#21874 = ORIENTED_EDGE ( 'NONE', *, *, #21928, .F. ) ;
#21875 = CARTESIAN_POINT ( 'NONE',  ( 4.603870848087811218, 30.13529352683433515, -225.9623629403671430 ) ) ;
#21876 = CARTESIAN_POINT ( 'NONE',  ( 22.50501984129641286, -15.15275112778533284, -228.8333022290248664 ) ) ;
#21877 = CARTESIAN_POINT ( 'NONE',  ( 0.000000000000000000, 0.000000000000000000, -24.99999999999999645 ) ) ;
#21878 = CARTESIAN_POINT ( 'NONE',  ( 0.000000000000000000, 0.000000000000000000, 77.51594804401857175 ) ) ;
#21879 = CARTESIAN_POINT ( 'NONE',  ( 4.340445191644851874, 29.86837761166362881, -227.4879512554873315 ) ) ;
#21880 = CARTESIAN_POINT ( 'NONE',  ( -8.215923615656011592, -19.99105411527736820, -235.1422105638354481 ) ) ;
#21881 = CARTESIAN_POINT ( 'NONE',  ( 1.752757082432757185, -17.15725705531007250, -232.7539178101738742 ) ) ;
#21882 = CARTESIAN_POINT ( 'NONE',  ( 0.000000000000000000, 0.000000000000000000, -69.99999999999998579 ) ) ;
#21883 = CARTESIAN_POINT ( 'NONE',  ( -9.982417347796181062, 8.907629238417765549, -225.5124013436514474 ) ) ;
#21884 = CARTESIAN_POINT ( 'NONE',  ( 8.961491954973460849, 17.27041174997091844, -219.7661252763212474 ) ) ;
#21885 = CARTESIAN_POINT ( 'NONE',  ( -29.95012366401462955, 4.746560250930182967, -224.6954343660969471 ) ) ;
#21886 = CARTESIAN_POINT ( 'NONE',  ( -21.29946384424354733, 21.01772963953914442, -222.5871995662667757 ) ) ;
#21887 = CARTESIAN_POINT ( 'NONE',  ( -20.80379704402785990, -7.385557752804055909, -217.9407440132496845 ) ) ;
#21888 = EDGE_CURVE ( 'NONE', #9986, #16736, #19588, .T. ) ;
#21889 = CARTESIAN_POINT ( 'NONE',  ( -10.70754874174748039, 23.84972878377777405, -230.7991598016655246 ) ) ;
#21890 = CARTESIAN_POINT ( 'NONE',  ( 12.88374853655145458, 4.106359831454843068, -228.1016120772327440 ) ) ;
#21891 = CARTESIAN_POINT ( 'NONE',  ( 2.804048525646705148, 30.59371477727813726, -220.6614663749232363 ) ) ;
#21892 = CARTESIAN_POINT ( 'NONE',  ( 17.56598174185312899, -13.96259959359126768, -216.8519506175684626 ) ) ;
#21893 = CARTESIAN_POINT ( 'NONE',  ( 0.000000000000000000, 0.000000000000000000, -25.00000000000000000 ) ) ;
#21894 = ORIENTED_EDGE ( 'NONE', *, *, #7097, .F. ) ;
#21895 = CARTESIAN_POINT ( 'NONE',  ( -25.80904414196669450, 12.19501778665756220, -219.1732313092283846 ) ) ;
#21896 = CARTESIAN_POINT ( 'NONE',  ( -12.51550321509044927, -6.200974036110347143, -231.2371560537167170 ) ) ;
#21897 = DIRECTION ( 'NONE',  ( 1.000000000000000000, 0.000000000000000000, -0.000000000000000000 ) ) ;
#21898 = CARTESIAN_POINT ( 'NONE',  ( 8.496844655769807630, 14.66037471857024599, -219.1631158796573118 ) ) ;
#21899 = FACE_BOUND ( 'NONE', #15657, .T. ) ;
#21900 = CARTESIAN_POINT ( 'NONE',  ( 14.90979066288448429, -1.927202206923867234, -222.7790985701595616 ) ) ;
#21901 = FILL_AREA_STYLE ('',( #1322 ) ) ;
#21902 = CARTESIAN_POINT ( 'NONE',  ( -13.98136146596813845, 3.850743984385103680, -228.7620665878280590 ) ) ;
#21903 = CARTESIAN_POINT ( 'NONE',  ( -11.39536650977235510, 9.246300577217761330, -228.4898727004871546 ) ) ;
#21904 = CARTESIAN_POINT ( 'NONE',  ( 17.47660375112063491, 0.1533180678384444551, -220.6249646429494931 ) ) ;
#21905 =( NAMED_UNIT ( * ) SI_UNIT ( $, .STERADIAN. ) SOLID_ANGLE_UNIT ( ) );
#21906 = CARTESIAN_POINT ( 'NONE',  ( 15.41510009650066770, 0.5889348971793676446, -222.0565507956523277 ) ) ;
#21907 = CARTESIAN_POINT ( 'NONE',  ( 18.46552355142154411, 5.019711608606525211, -231.5099115070375433 ) ) ;
#21908 = CARTESIAN_POINT ( 'NONE',  ( -21.89482327431018760, 1.733733432562314158, -233.1353281693111796 ) ) ;
#21909 = CARTESIAN_POINT ( 'NONE',  ( 15.34439776706934921, -6.609831973102724412, -222.6284221295667862 ) ) ;
#21910 = CARTESIAN_POINT ( 'NONE',  ( -28.18501077041064562, -8.523171531337160545, -227.0531053546762337 ) ) ;
#21911 = CARTESIAN_POINT ( 'NONE',  ( -20.83653394098313427, -9.738788406788492225, 2.294410813807128413 ) ) ;
#21912 = CARTESIAN_POINT ( 'NONE',  ( 1.665334536937734811E-13, -24.63401512838747820, 77.51594804401857175 ) ) ;
#21913 = CARTESIAN_POINT ( 'NONE',  ( 0.07890756785233743464, 25.14108539708653822, -218.4152285319504756 ) ) ;
#21914 = CARTESIAN_POINT ( 'NONE',  ( 13.82710435306955432, -11.68840971183345800, -215.7775723145259974 ) ) ;
#21915 = CARTESIAN_POINT ( 'NONE',  ( 6.260999666360449467, -13.19315344885661645, -220.2890618333529744 ) ) ;
#21916 = CARTESIAN_POINT ( 'NONE',  ( -13.51406939156936104, 10.04301168678160749, -230.1761202643687056 ) ) ;
#21917 = CARTESIAN_POINT ( 'NONE',  ( 17.91327661571172314, 1.545939370248587075, -216.9938266089438912 ) ) ;
#21918 = CARTESIAN_POINT ( 'NONE',  ( 16.26115440404298340, 3.800605480264513059, -219.2833057824682612 ) ) ;
#21919 = ORIENTED_EDGE ( 'NONE', *, *, #16995, .F. ) ;
#21920 = CARTESIAN_POINT ( 'NONE',  ( -1.178362239076253370, -26.64461120719161613, -230.8441371545519019 ) ) ;
#21921 = DIRECTION ( 'NONE',  ( 1.401298464324817071E-45, 6.938893903907257960E-16, -1.000000000000000000 ) ) ;
#21922 = CARTESIAN_POINT ( 'NONE',  ( -23.68377094563794572, 13.02263794644603578, -215.9752901280847652 ) ) ;
#21923 = CARTESIAN_POINT ( 'NONE',  ( 7.803634760976553508, 10.78293796201124266, -229.6314106675118865 ) ) ;
#21924 = CARTESIAN_POINT ( 'NONE',  ( -0.04850409037381671340, 14.20520396026658716, -231.8092226852533031 ) ) ;
#21925 = CARTESIAN_POINT ( 'NONE',  ( 23.00003818093501806, -2.342406833639917085, -233.2756072794339843 ) ) ;
#21926 = CARTESIAN_POINT ( 'NONE',  ( 5.069241901512100412, 14.34986542013820632, -229.6420000777802954 ) ) ;
#21927 = CARTESIAN_POINT ( 'NONE',  ( -18.46722752239034193, 0.9784074152395518809, -232.1633353206286188 ) ) ;
#21928 = EDGE_CURVE ( 'NONE', #15746, #12201, #16752, .T. ) ;
#21929 = CARTESIAN_POINT ( 'NONE',  ( 9.169328349715531346, 20.85917603618721472, -214.7000934853629133 ) ) ;
#21930 = CARTESIAN_POINT ( 'NONE',  ( -17.91550223652134122, 4.809113705933536487, -230.6324822114035555 ) ) ;
#21931 = CARTESIAN_POINT ( 'NONE',  ( -10.45786516112131892, 23.61456281964591852, -233.2869923610001592 ) ) ;
#21932 = CARTESIAN_POINT ( 'NONE',  ( 15.01439307471096463, 1.118969480519667048, -226.7488225241675366 ) ) ;
#21933 = CARTESIAN_POINT ( 'NONE',  ( 15.28499842775873319, 22.98894588155567931, -221.0942409093412095 ) ) ;
#21934 = CARTESIAN_POINT ( 'NONE',  ( 0.000000000000000000, 0.000000000000000000, -77.51594804401857175 ) ) ;
#21935 = DIRECTION ( 'NONE',  ( 0.000000000000000000, 0.000000000000000000, -1.000000000000000000 ) ) ;
#21936 = CARTESIAN_POINT ( 'NONE',  ( -17.92628912275201003, -0.6090139417824500523, -215.7724435048976943 ) ) ;
#21937 = CARTESIAN_POINT ( 'NONE',  ( -14.27403737459813193, -10.90264666745762057, -220.2309642783388597 ) ) ;
#21938 = CARTESIAN_POINT ( 'NONE',  ( 2.999999999999971578, 3.673940397442062826E-16, -221.9999999999999716 ) ) ;
#21939 = CARTESIAN_POINT ( 'NONE',  ( -9.233762381136051189, 19.18161952504991419, -232.0796851897838451 ) ) ;
#21940 = SURFACE_STYLE_USAGE ( .BOTH. , #11601 ) ;
#21941 = CARTESIAN_POINT ( 'NONE',  ( 6.869068212838696397, -24.78254998730118430, -231.2855974421026986 ) ) ;
#21942 = CARTESIAN_POINT ( 'NONE',  ( 23.08329078023534109, 11.96623404944238978, -217.1428499060670845 ) ) ;
#21943 = CARTESIAN_POINT ( 'NONE',  ( -12.67219131930435694, 19.52425521811199971, -218.0046184995277372 ) ) ;
#21944 = CARTESIAN_POINT ( 'NONE',  ( -8.201407585998298444, 17.38801480109368924, -216.6295241303755006 ) ) ;
#21945 = ORIENTED_EDGE ( 'NONE', *, *, #9938, .F. ) ;
#21946 = CARTESIAN_POINT ( 'NONE',  ( -23.94935377092574669, -14.34094158514532680, -226.5194954081123342 ) ) ;
#21947 = CARTESIAN_POINT ( 'NONE',  ( 8.329997790135040603, 12.51216704542961899, -228.7022893680961602 ) ) ;
#21948 = CARTESIAN_POINT ( 'NONE',  ( -18.88344489807484905, 1.071113352238720617, -230.0966926586188208 ) ) ;
#21949 = CARTESIAN_POINT ( 'NONE',  ( -3.000000000000033751, 0.000000000000000000, -227.9999999999999716 ) ) ;
#21950 = CARTESIAN_POINT ( 'NONE',  ( -23.51371042417668633, 2.081716773471995463, -216.9231029201042418 ) ) ;
#21951 = CARTESIAN_POINT ( 'NONE',  ( 17.97920459523930958, 17.43922474653955490, -233.2737719749805763 ) ) ;
#21952 = MANIFOLD_SOLID_BREP ( 'Cavity1', #9021 ) ;
#21953 = CARTESIAN_POINT ( 'NONE',  ( -15.82760502346409304, 5.624826830110399634, -227.5369622385896946 ) ) ;
#21954 = CARTESIAN_POINT ( 'NONE',  ( 0.1866476013601106043, 25.93503619265524307, -233.5574764272258790 ) ) ;
#21955 = CARTESIAN_POINT ( 'NONE',  ( 27.58248235015124550, 10.80791576765187934, -226.6933256641281389 ) ) ;
#21956 = ORIENTED_EDGE ( 'NONE', *, *, #1440, .F. ) ;
#21957 = CARTESIAN_POINT ( 'NONE',  ( -17.08385316318651448, -18.56764924811779949, -215.7277288032969977 ) ) ;
#21958 = ORIENTED_EDGE ( 'NONE', *, *, #1722, .F. ) ;
#21959 = CARTESIAN_POINT ( 'NONE',  ( -11.18311023676720062, -15.30649302686804347, -231.8766562234714002 ) ) ;
#21960 = CARTESIAN_POINT ( 'NONE',  ( -20.02994071726468661, 1.326980477106467271, -234.9527056834518532 ) ) ;
#21961 = CARTESIAN_POINT ( 'NONE',  ( 6.131461862964278531, -15.14974102410872625, -231.6805438559109973 ) ) ;
#21962 = CARTESIAN_POINT ( 'NONE',  ( 14.15946391865398013, -0.7413617426029489588, -228.5799580636366670 ) ) ;
#21963 = CARTESIAN_POINT ( 'NONE',  ( -16.20471097821853235, -2.781505378741172319, -220.1484675126197317 ) ) ;
#21964 = CARTESIAN_POINT ( 'NONE',  ( 26.39436175479395885, 14.32821500273865034, -221.6819523832376149 ) ) ;
#21965 = PRESENTATION_STYLE_ASSIGNMENT (( #13430 ) ) ;
#21966 = CARTESIAN_POINT ( 'NONE',  ( -15.63515374589483109, 24.59141623553136569, -226.9057426066772507 ) ) ;
#21967 = CARTESIAN_POINT ( 'NONE',  ( 13.60311248493089131, 7.003372205918751092, -219.1738832909067867 ) ) ;
#21968 = CARTESIAN_POINT ( 'NONE',  ( 21.25094435758043332, 17.68230636442804027, -229.7964888993842010 ) ) ;
#21969 = CARTESIAN_POINT ( 'NONE',  ( 10.49810582199713416, 9.357428619962972149, -224.5466107281195605 ) ) ;
#21970 = CARTESIAN_POINT ( 'NONE',  ( 26.45187990207246997, -15.96729416691344383, -220.4105496189887674 ) ) ;
#21971 = CARTESIAN_POINT ( 'NONE',  ( -8.892156391762910062, 11.89593067802204551, -225.4519868197583889 ) ) ;
#21972 = PRODUCT_DEFINITION_SHAPE ( 'NONE', 'NONE',  #22272 ) ;
#21973 = CARTESIAN_POINT ( 'NONE',  ( -15.23434562258889891, -0.4010941804143903222, -220.4743703065900036 ) ) ;
#21974 = DIRECTION ( 'NONE',  ( -1.000000000000000000, 0.000000000000000000, 0.000000000000000000 ) ) ;
#21975 = VECTOR ( 'NONE', #5125, 1000.000000000000000 ) ;
#21976 = CARTESIAN_POINT ( 'NONE',  ( 16.84848658399567611, 11.39632653812981644, -217.9589513831453473 ) ) ;
#21977 = CARTESIAN_POINT ( 'NONE',  ( 4.470318609411144450, -14.75491745724135306, -219.7618428768379886 ) ) ;
#21978 = CARTESIAN_POINT ( 'NONE',  ( -24.18895665211001500, 11.26087434487096139, -231.0040666710689550 ) ) ;
#21979 = CARTESIAN_POINT ( 'NONE',  ( 3.080453011304693511, 29.32691491905673331, -222.8956499783474499 ) ) ;
#21980 = CARTESIAN_POINT ( 'NONE',  ( -18.44715843167851688, -19.86029123650958184, -231.9563062773970046 ) ) ;
#21981 = ITEM_DEFINED_TRANSFORMATION ( 'NONE', 'NONE', #19270,  #6677 ) ;
#21982 = CARTESIAN_POINT ( 'NONE',  ( -18.46822229429615447, 3.027586163204024405, -230.1002726880134333 ) ) ;
#21983 = CIRCLE ( 'NONE', #21257, 1.000000000000000888 ) ;
#21984 = CARTESIAN_POINT ( 'NONE',  ( 12.92410717862594893, 29.37236178718849189, -224.5435071569520744 ) ) ;
#21985 = ORIENTED_EDGE ( 'NONE', *, *, #1596, .T. ) ;
#21986 = CARTESIAN_POINT ( 'NONE',  ( -2.934221234790329369, 15.07857928364152222, -230.9558365497803720 ) ) ;
#21987 = CARTESIAN_POINT ( 'NONE',  ( 17.03334375980016446, -6.184066897328505341, -231.2622903164569834 ) ) ;
#21988 = CARTESIAN_POINT ( 'NONE',  ( 24.64273247744971229, -10.07127014888436278, -217.7281412196979602 ) ) ;
#21989 = DIRECTION ( 'NONE',  ( 0.000000000000000000, 0.000000000000000000, 1.000000000000000000 ) ) ;
#21990 = CARTESIAN_POINT ( 'NONE',  ( -0.3969026096611234511, 20.89748314411456676, -216.3289738411752978 ) ) ;
#21991 = CARTESIAN_POINT ( 'NONE',  ( -26.37829495954481374, -14.45191861565034053, -218.9345690753252711 ) ) ;
#21992 = CARTESIAN_POINT ( 'NONE',  ( 14.65870393774896030, -26.09170264574407838, -221.2973805112574723 ) ) ;
#21993 = CARTESIAN_POINT ( 'NONE',  ( 12.31511859722645852, -8.491226738247512174, -220.9006323875693738 ) ) ;
#21994 = CARTESIAN_POINT ( 'NONE',  ( -15.72555926117677139, 17.60926865496976745, -217.2114552733360142 ) ) ;
#21995 = CARTESIAN_POINT ( 'NONE',  ( 9.653903571287008489, 19.16609876806546353, -219.1149796918802792 ) ) ;
#21996 = CARTESIAN_POINT ( 'NONE',  ( -12.44873260470819787, 7.411970124596155785, -229.4214091473984070 ) ) ;
#21997 = CARTESIAN_POINT ( 'NONE',  ( -12.10258892854866275, 5.599955477755926836, -221.6590149575334010 ) ) ;
#21998 = CARTESIAN_POINT ( 'NONE',  ( -12.22799442060091657, -11.48557521842085372, -222.2662941369099201 ) ) ;
#21999 = ORIENTED_EDGE ( 'NONE', *, *, #15715, .T. ) ;
#22000 = AXIS2_PLACEMENT_3D ( 'NONE', #1906, #3589, #15651 ) ;
#22001 = CARTESIAN_POINT ( 'NONE',  ( -8.407534899841293097, 16.91942258446019665, -231.3029992963236339 ) ) ;
#22002 = CARTESIAN_POINT ( 'NONE',  ( 11.96568375430165254, 8.504117401580989721, -219.8633768076029753 ) ) ;
#22003 = CARTESIAN_POINT ( 'NONE',  ( 0.1866476013601106043, 25.93503619265524307, -233.5574764272258790 ) ) ;
#22004 = CARTESIAN_POINT ( 'NONE',  ( 15.56514059923893178, -9.210181625211102840, -232.5361143517874325 ) ) ;
#22005 = ORIENTED_EDGE ( 'NONE', *, *, #8163, .F. ) ;
#22006 = CARTESIAN_POINT ( 'NONE',  ( -17.17400284685640344, 24.63223427531467280, -220.6313524368512162 ) ) ;
#22007 = CARTESIAN_POINT ( 'NONE',  ( -15.10499565381530118, -6.968761303117489980, -233.6783966751926869 ) ) ;
#22008 = CARTESIAN_POINT ( 'NONE',  ( 0.000000000000000000, 21.00000000000006040, -69.99999999999998579 ) ) ;
#22009 = CARTESIAN_POINT ( 'NONE',  ( 15.33737796850231305, 13.57479350230705428, -232.3313557812109025 ) ) ;
#22010 = FACE_OUTER_BOUND ( 'NONE', #10231, .T. ) ;
#22011 = UNCERTAINTY_MEASURE_WITH_UNIT (LENGTH_MEASURE( 1.000000000000000082E-05 ), #2998, 'distance_accuracy_value', 'NONE');
#22012 = CARTESIAN_POINT ( 'NONE',  ( 12.84024077373997841, -14.50125846907313054, -216.8496453050001946 ) ) ;
#22013 = SURFACE_STYLE_USAGE ( .BOTH. , #11674 ) ;
#22014 = CARTESIAN_POINT ( 'NONE',  ( -20.43618815875133521, 1.403378831510147196, -232.9646741665398224 ) ) ;
#22015 = CARTESIAN_POINT ( 'NONE',  ( -8.413706464639300719, 10.92140547936800843, -220.6417935981040728 ) ) ;
#22016 = AXIS2_PLACEMENT_3D ( 'NONE', #20081, #13013, #6139 ) ;
#22017 = EDGE_CURVE ( 'NONE', #17384, #16873, #9929, .T. ) ;
#22018 = CARTESIAN_POINT ( 'NONE',  ( 20.88210880980788531, 0.9259446317980322139, -218.6312544800709929 ) ) ;
#22019 = EDGE_CURVE ( 'NONE', #21036, #10050, #1289, .T. ) ;
#22020 = CARTESIAN_POINT ( 'NONE',  ( -6.266309075335420253, -15.78290365675015572, -230.2363798222519051 ) ) ;
#22021 = CIRCLE ( 'NONE', #19509, 23.00000000000000000 ) ;
#22022 = FACE_OUTER_BOUND ( 'NONE', #20450, .T. ) ;
#22023 = CARTESIAN_POINT ( 'NONE',  ( 17.07668571305246985, 2.037405138410691485, -219.7626854147787867 ) ) ;
#22024 = CARTESIAN_POINT ( 'NONE',  ( 0.000000000000000000, 0.000000000000000000, -103.0000000000000000 ) ) ;
#22025 = CARTESIAN_POINT ( 'NONE',  ( 20.43533161254376296, -19.75510188685668567, -224.2614117135439074 ) ) ;
#22026 = CARTESIAN_POINT ( 'NONE',  ( -26.22594988380878789, -0.1068133454905619700, -219.1167922977186322 ) ) ;
#22027 = CARTESIAN_POINT ( 'NONE',  ( -21.58840139808157232, -7.942961002574626228, 6.109722015442944354 ) ) ;
#22028 = DIRECTION ( 'NONE',  ( 0.000000000000000000, 0.000000000000000000, -1.000000000000000000 ) ) ;
#22029 = CARTESIAN_POINT ( 'NONE',  ( 10.89019654021101857, 23.08162452736882031, -220.1893104909416934 ) ) ;
#22030 = CARTESIAN_POINT ( 'NONE',  ( 9.167096742983094515, -14.53852251116023986, -217.0563232478103828 ) ) ;
#22031 = CARTESIAN_POINT ( 'NONE',  ( 11.78320976064766690, -8.193118641535518165, -222.2581747538435479 ) ) ;
#22032 = ORIENTED_EDGE ( 'NONE', *, *, #2399, .F. ) ;
#22033 = CARTESIAN_POINT ( 'NONE',  ( -22.24722865165759345, 18.77558306771206986, -226.5077042908023941 ) ) ;
#22034 = CARTESIAN_POINT ( 'NONE',  ( 17.23498165643884761, 6.576565757823654934, -216.5785374982484655 ) ) ;
#22035 = CARTESIAN_POINT ( 'NONE',  ( 19.31922195716811430, 9.600631919686000160, -218.1359845693048101 ) ) ;
#22036 = EDGE_LOOP ( 'NONE', ( #8555, #15302, #5993, #16137 ) ) ;
#22037 = CARTESIAN_POINT ( 'NONE',  ( -10.06242375715308945, -19.11710762076843295, -231.0938065448402199 ) ) ;
#22038 = MANIFOLD_SOLID_BREP ( 'Revolve1', #12174 ) ;
#22039 = DIRECTION ( 'NONE',  ( 0.000000000000000000, 0.000000000000000000, 1.000000000000000000 ) ) ;
#22040 = CIRCLE ( 'NONE', #2625, 19.63401512838747820 ) ;
#22041 = CARTESIAN_POINT ( 'NONE',  ( -21.85741505224184777, 1.741064654082184582, -235.1654459941842390 ) ) ;
#22042 = CIRCLE ( 'NONE', #15594, 3.000000000000002665 ) ;
#22043 = CARTESIAN_POINT ( 'NONE',  ( 17.88619020626327938, 19.43517936004721847, -216.7078103882350604 ) ) ;
#22044 = CARTESIAN_POINT ( 'NONE',  ( 9.413533971304945069, -13.52850967935795623, -226.9656141048783695 ) ) ;
#22045 = CARTESIAN_POINT ( 'NONE',  ( 5.623554730548537606, 15.65270319720736225, -231.3185741195121068 ) ) ;
#22046 = CARTESIAN_POINT ( 'NONE',  ( -22.11084984981285118, 10.96048252433489623, -216.6117774006995376 ) ) ;
#22047 = CARTESIAN_POINT ( 'NONE',  ( 5.434119414999338815, 11.18343085245738777, -221.0450680983404936 ) ) ;
#22048 = EDGE_CURVE ( 'NONE', #4211, #17072, #13885, .T. ) ;
#22049 = CARTESIAN_POINT ( 'NONE',  ( -18.63458318964815774, 8.046101765467303935, -217.8151248213926863 ) ) ;
#22050 = CARTESIAN_POINT ( 'NONE',  ( -7.913358619554302642, 16.16796202616373890, -233.0981776325470491 ) ) ;
#22051 = CARTESIAN_POINT ( 'NONE',  ( 18.60971343765040942, 2.368090295052050820, -218.6871071987073094 ) ) ;
#22052 = CIRCLE ( 'NONE', #12370, 21.80000000000000071 ) ;
#22053 = CARTESIAN_POINT ( 'NONE',  ( 2.659252340503933443, 26.58135124637517777, -228.4751214701929314 ) ) ;
#22054 = CARTESIAN_POINT ( 'NONE',  ( 0.000000000000000000, 0.000000000000000000, 75.00000000000000000 ) ) ;
#22055 = CYLINDRICAL_SURFACE ( 'NONE', #17094, 3.000000000000002665 ) ;
#22056 = CARTESIAN_POINT ( 'NONE',  ( -19.88402822078561627, -6.951120502836210413, -232.7962440186676361 ) ) ;
#22057 = CARTESIAN_POINT ( 'NONE',  ( -22.61701582078733708, 5.416317966792455252, -214.6955127214549748 ) ) ;
#22058 = CARTESIAN_POINT ( 'NONE',  ( -20.64589292112740537, -18.79971917946562598, -222.0410088502282520 ) ) ;
#22059 = CARTESIAN_POINT ( 'NONE',  ( 22.00000000000000000, 6.162975822039154730E-30, -228.0000000000000000 ) ) ;
#22060 = CARTESIAN_POINT ( 'NONE',  ( -8.317278876689359279, 23.15034512777772235, -218.2935523245793092 ) ) ;
#22061 = CARTESIAN_POINT ( 'NONE',  ( 1.874647746501092893, -15.20125101474619633, -222.7462710229423521 ) ) ;
#22062 = EDGE_CURVE ( 'NONE', #6505, #7331, #7780, .T. ) ;
#22063 = CARTESIAN_POINT ( 'NONE',  ( 10.14297843322460402, 14.69845403004500639, -219.2805000163441207 ) ) ;
#22064 = CARTESIAN_POINT ( 'NONE',  ( -8.030397104878142400, 15.90963402996711373, -230.6518438502475590 ) ) ;
#22065 = CARTESIAN_POINT ( 'NONE',  ( -14.12265793148702464, 24.49085167151569919, -218.3312790639385241 ) ) ;
#22066 = ORIENTED_EDGE ( 'NONE', *, *, #22215, .T. ) ;
#22067 = CARTESIAN_POINT ( 'NONE',  ( -15.75487091793989158, -3.404709188850186585, -225.0852311470768825 ) ) ;
#22068 = CARTESIAN_POINT ( 'NONE',  ( 18.23324537670537993, 23.47692953258263771, -224.8333321331434433 ) ) ;
#22069 = CARTESIAN_POINT ( 'NONE',  ( -25.06333669508177309, 2.553070212212491530, -230.2963116797556893 ) ) ;
#22070 = CARTESIAN_POINT ( 'NONE',  ( -27.01279207917464475, 4.316569700791554887, -221.4451031230926219 ) ) ;
#22071 = ADVANCED_FACE ( 'NONE', ( #13996 ), #5414, .F. ) ;
#22072 = DIRECTION ( 'NONE',  ( 0.000000000000000000, 0.000000000000000000, -1.000000000000000000 ) ) ;
#22073 = CARTESIAN_POINT ( 'NONE',  ( -26.70887854271809658, -5.532318215328999145, -217.2738835169348306 ) ) ;
#22074 = CARTESIAN_POINT ( 'NONE',  ( 17.29648694364601980, 10.20782262162153842, -233.8400727604031317 ) ) ;
#22075 = CIRCLE ( 'NONE', #152, 19.79999999999999716 ) ;
#22076 = CARTESIAN_POINT ( 'NONE',  ( -15.32935061426341861, 5.146212415319166844, -225.5669090095357774 ) ) ;
#22077 = CARTESIAN_POINT ( 'NONE',  ( 11.13671218404335761, 30.21738803452449673, -224.2405745632392211 ) ) ;
#22078 = CARTESIAN_POINT ( 'NONE',  ( 14.65697969206133067, 11.40587726087447606, -233.3943609825344652 ) ) ;
#22079 = CARTESIAN_POINT ( 'NONE',  ( -13.20345004609422723, -27.40577205094947644, -221.7016714442654290 ) ) ;
#22080 = ORIENTED_EDGE ( 'NONE', *, *, #19998, .T. ) ;
#22081 = CARTESIAN_POINT ( 'NONE',  ( -4.879290506874147226, -14.18937706998098136, -223.0759034783553147 ) ) ;
#22082 = CARTESIAN_POINT ( 'NONE',  ( -14.74212732455322161, 0.2624230007780231633, -231.8143822214177874 ) ) ;
#22083 = CARTESIAN_POINT ( 'NONE',  ( 2.178520447619924472, -13.56847537563065487, -221.4085897031499428 ) ) ;
#22084 = CARTESIAN_POINT ( 'NONE',  ( -10.84997096467605182, 25.01800101807719301, -232.4518260228253155 ) ) ;
#22085 = CARTESIAN_POINT ( 'NONE',  ( 17.72923050078999907, -1.936365952008033853, -232.4832991314195567 ) ) ;
#22086 = CARTESIAN_POINT ( 'NONE',  ( -15.89118508636071958, -1.798691612803976492, -229.3605869667087234 ) ) ;
#22087 = CARTESIAN_POINT ( 'NONE',  ( 12.14863411169100971, 10.95505907656739097, -219.3725293661985063 ) ) ;
#22088 = CARTESIAN_POINT ( 'NONE',  ( 0.000000000000000000, 0.000000000000000000, -103.0000000000000000 ) ) ;
#22089 = CARTESIAN_POINT ( 'NONE',  ( -10.94147694953847250, 13.90730769817462864, -218.7797619932150042 ) ) ;
#22090 = CARTESIAN_POINT ( 'NONE',  ( 13.88312867625433711, 12.44451767566605760, -217.7066242262208391 ) ) ;
#22091 = AXIS2_PLACEMENT_3D ( 'NONE', #6304, #17609, #13178 ) ;
#22092 = CARTESIAN_POINT ( 'NONE',  ( 10.83706092800007781, 10.12544885278926543, -227.1716144446442343 ) ) ;
#22093 = CARTESIAN_POINT ( 'NONE',  ( 12.63974878616558328, 15.03448928898568759, -231.7036488814491406 ) ) ;
#22094 = CARTESIAN_POINT ( 'NONE',  ( 7.292867580403318506, -17.79718201325288263, -215.1213547356373397 ) ) ;
#22095 = STYLED_ITEM ( 'NONE', ( #19769 ), #5876 ) ;
#22096 = CARTESIAN_POINT ( 'NONE',  ( -12.66290653391502907, 23.44312233264792411, -230.9359094203250606 ) ) ;
#22097 = LINE ( 'NONE', #20061, #14446 ) ;
#22098 = CARTESIAN_POINT ( 'NONE',  ( 10.76794919243112325, 0.000000000000000000, 92.50000000000000000 ) ) ;
#22099 = DIRECTION ( 'NONE',  ( -1.000000000000000000, 0.000000000000000000, 0.000000000000000000 ) ) ;
#22100 = CARTESIAN_POINT ( 'NONE',  ( 9.471595414968767557, -23.22249338881061931, -232.1368331642201497 ) ) ;
#22101 = CARTESIAN_POINT ( 'NONE',  ( -22.04240660558204823, 19.10355008918698871, -223.9524535985323723 ) ) ;
#22102 = B_SPLINE_CURVE_WITH_KNOTS ( 'NONE', 3,
 ( #968, #11538, #4556, #16498, #16279, #8175, #13340, #2649, #9859, #14708, #16724, #18078, #17973, #854, #4665, #7949, #14602, #2537, #4226, #1301, #15041, #9636, #21543, #11105, #9530, #7731, #6133, #21437, #6027, #13007, #12901, #19748, #19969, #4440, #9745, #11323, #18192, #2755, #14813, #11432, #21658, #6249, #13123, #18301, #16607, #2860, #1189, #8067, #14932, #21771, #6360, #13232, #20078, #21993, #17061, #20412, #5108, #1410, #16946, #17168, #173, #7042, #10414, #4777, #20637, #3198, #20297, #10081, #17275, #3534, #12103, #11990, #20182, #3090, #18741, #13457, #18850, #11877, #8515, #8727, #5222, #9973, #10305, #15268, #1849, #3425, #10192, #15593, #11653, #18524, #1746, #16833, #3308, #6587, #13576, #8282, #4892, #15151, #18636, #11772, #1522, #18958, #8400, #22118, #6705, #5001, #1638, #15378, #22225, #6816, #13682, #20518, #8620, #15481, #54, #6927, #13797, #17506, #14135, #19065, #12546, #1965, #2401, #19178, #16143, #17613, #14355, #2073, #15709, #3640, #715, #7265, #2179, #20857, #5561, #10850, #9060, #19500, #21187, #20974, #13914, #5773, #16039, #20749, #394, #611, #12212, #12654, #14021, #2291, #19290, #10639, #4089, #5441, #10521, #12323, #10965, #17836, #3754, #9283, #17390, #8843, #5330, #7155, #15926, #7486, #8953, #286, #17724, #15817, #12439, #3867, #10747, #19393, #504, #7380, #14248, #21081, #5668, #3976, #9176, #11405, #11077, #12764, #17944, #2508, #4300, #4410, #16360, #937, #2835, #16691, #20050, #14458, #8035, #14680, #21514, #21741, #19825, #18164, #6332, #14785, #6106, #2728, #18380, #14901, #2618, #19613, #13093, #5998, #7702, #19720, #9830, #14572, #1048, #11292, #18274, #12871, #7589, #2943, #7921, #823, #9386, #11182, #21291, #4637, #21626, #6218, #19940, #1159, #9499, #4198, #5887, #16248, #21408, #9717, #18049, #7815, #12977, #16578, #16471, #9609, #4527, #13205, #11511, #22200, #21852, #18825, #8489, #18933, #1493, #18610, #6899, #12077, #20608, #20269, #8596, #1610, #13548, #6441, #5194, #18717, #13769, #15457, #16919, #10387, #8371, #30, #3397, #1272, #10056, #10279, #13310, #3508, #1381, #11964, #6676, #4865, #8147, #15124, #20152, #15352, #15012, #11742, #20383, #4977, #17145, #4745, #11624, #16806, #3281, #1721, #21963, #18496, #20493, #3172, #3057, #9946, #15241, #6788, #22086, #8257, #11852, #6556, #10166, #13428, #17035, #5083, #13657, #143, #20721, #5302, #13994, #14107, #5411, #16009, #1936, #8697 ),
 .UNSPECIFIED., .F., .F.,
 ( 4, 2, 2, 2, 2, 2, 2, 2, 2, 2, 2, 2, 2, 2, 2, 2, 2, 2, 2, 2, 2, 2, 2, 2, 2, 2, 2, 2, 2, 2, 2, 2, 2, 2, 2, 2, 2, 2, 2, 2, 2, 2, 2, 2, 2, 2, 2, 2, 2, 2, 2, 2, 2, 2, 2, 2, 2, 2, 2, 2, 2, 2, 2, 2, 2, 2, 2, 2, 2, 2, 2, 2, 2, 2, 2, 2, 2, 2, 2, 2, 2, 2, 2, 2, 2, 2, 2, 2, 2, 2, 2, 2, 2, 2, 2, 2, 2, 2, 2, 2, 2, 2, 2, 2, 2, 2, 2, 2, 2, 2, 2, 2, 2, 2, 2, 2, 2, 2, 2, 2, 2, 2, 2, 2, 2, 2, 2, 2, 2, 2, 2, 2, 2, 2, 2, 2, 2, 2, 2, 2, 2, 2, 2, 2, 2, 2, 2, 2, 2, 2, 2, 2, 2, 2, 2, 2, 2, 2, 4 ),
 ( 0.5316166001436728461, 0.5336398250262029963, 0.5353489984423374093, 0.5370581718584717112, 0.5404765186907403152, 0.5438948655230090301, 0.5473132123552777450, 0.5507315591875463490, 0.5541499060198149529, 0.5575682528520836678, 0.5609865996843523828, 0.5644049465166209867, 0.5661141199327552886, 0.5678232933488895906, 0.5712416401811581945, 0.5729508135972924965, 0.5746599870134267984, 0.5780783338456955134, 0.5814966806779642283, 0.5849150275102328322, 0.5883333743425015472, 0.5917517211747702621, 0.5951700680070388660, 0.5985884148393075810, 0.6020067616715762959, 0.6037159350877105979, 0.6054251085038448998, 0.6088434553361135038, 0.6122618021683822187, 0.6139709755845166317, 0.6156801490006509336, 0.6190984958329195376, 0.6225168426651882525, 0.6259351894974569674, 0.6293535363297255714, 0.6327718831619942863, 0.6361902299942630012, 0.6396085768265316052, 0.6430269236588003201, 0.6447360970749347331, 0.6464452704910690350, 0.6498636173233376390, 0.6532819641556063539, 0.6549911375717407669, 0.6567003109878750688, 0.6601186578201436728, 0.6635370046524122767, 0.6669553514846809916, 0.6703736983169497066, 0.6737920451492183105, 0.6772103919814870254, 0.6806287388137557404, 0.6840470856460243443, 0.6857562590621586462, 0.6866108457702257972, 0.6874654324782930592, 0.6908837793105617742, 0.6943021261428303781, 0.6960112995589646800, 0.6977204729750989820, 0.7011388198073676969, 0.7045571666396364119, 0.7079755134719050158, 0.7113938603041736197, 0.7148122071364423347, 0.7182305539687110496, 0.7216489008009796535, 0.7250672476332483685, 0.7267764210493827814, 0.7284855944655170834, 0.7319039412977856873, 0.7353222881300544023, 0.7387406349623231172, 0.7421589817945917211, 0.7455773286268603250, 0.7489956754591290400, 0.7524140222913977549, 0.7558323691236663588, 0.7592507159559350738, 0.7626690627882037887, 0.7660874096204723926, 0.7695057564527411076, 0.7729241032850098225, 0.7763424501172784264, 0.7797607969495471414, 0.7831791437818158563, 0.7865974906140844602, 0.7900158374463531752, 0.7934341842786218901, 0.7968525311108904940, 0.8002708779431590980, 0.8036892247754278129, 0.8053983981915622259, 0.8071075716076965278, 0.8105259184399651318, 0.8122350918560994337, 0.8139442652722337357, 0.8173626121045024506, 0.8207809589367711656, 0.8241993057690397695, 0.8276176526013083734, 0.8310359994335770883, 0.8344543462658458033, 0.8378726930981144072, 0.8412910399303832332, 0.8430002133465175351, 0.8447093867626518371, 0.8481277335949204410, 0.8515460804271891559, 0.8549644272594578709, 0.8583827740917264748, 0.8618011209239951897, 0.8652194677562639047, 0.8686378145885325086, 0.8720561614208012235, 0.8754745082530699385, 0.8788928550853385424, 0.8823112019176071463, 0.8857295487498758613, 0.8874387221660102743, 0.8891478955821445762, 0.8925662424144131801, 0.8942754158305474821, 0.8959845892466818951, 0.8994029360789506100, 0.9028212829112192139, 0.9062396297434879289, 0.9096579765757566438, 0.9130763234080252477, 0.9164946702402939627, 0.9199130170725626776, 0.9233313639048312815, 0.9250405373209655835, 0.9267497107370999965, 0.9301680575693687114, 0.9335864044016373153, 0.9352955778177716173, 0.9370047512339059192, 0.9404230980661746342, 0.9438414448984433491, 0.9472597917307119531, 0.9506781385629806680, 0.9540964853952493829, 0.9575148322275179869, 0.9609331790597867018, 0.9643515258920554167, 0.9660606993081897187, 0.9677698727243240207, 0.9711882195565927356, 0.9728973929727271486, 0.9746065663888614505, 0.9780249132211300545, 0.9814432600533987694, 0.9848616068856674843, 0.9882799537179360883, 0.9912099652884520662, 0.9941399768589680441, 0.9970699884294840221, 1.000000000000000000 ),
 .UNSPECIFIED. ) ;
#22103 = CARTESIAN_POINT ( 'NONE',  ( 2.630208337444488453, 16.40323635460054774, -219.2570070657488088 ) ) ;
#22104 = CARTESIAN_POINT ( 'NONE',  ( -26.98579662683621194, -8.531126968542736222, -229.5232528995939845 ) ) ;
#22105 = CONTEXT_DEPENDENT_SHAPE_REPRESENTATION ( #1382, #3113 ) ;
#22106 = CARTESIAN_POINT ( 'NONE',  ( -17.64438593497130370, 2.824953307685432069, -229.4443205246391813 ) ) ;
#22108 = CARTESIAN_POINT ( 'NONE',  ( 22.90621760533471019, 17.25363305745006670, -230.8615280072714597 ) ) ;
#22107 = CIRCLE ( 'NONE', #11337, 22.56777165119825668 ) ;
#22109 = ORIENTED_EDGE ( 'NONE', *, *, #21540, .T. ) ;
#22110 = CARTESIAN_POINT ( 'NONE',  ( -11.02345917017863464, 29.02019856777526741, -223.9475008740665771 ) ) ;
#22111 = CARTESIAN_POINT ( 'NONE',  ( 27.02504508796729255, -10.76203424748690907, -225.6681254905965943 ) ) ;
#22112 = VECTOR ( 'NONE', #8373, 1000.000000000000000 ) ;
#22113 = CARTESIAN_POINT ( 'NONE',  ( 13.93061470302797389, -11.80544459979379646, -217.9389246709861538 ) ) ;
#22114 = LINE ( 'NONE', #11768, #14906 ) ;
#22115 = CARTESIAN_POINT ( 'NONE',  ( 0.9908753270255351575, 13.79205759140780430, -228.0165926715089881 ) ) ;
#22116 = CARTESIAN_POINT ( 'NONE',  ( -15.39182838237880446, -1.300641671086574469, -219.0680177603771597 ) ) ;
#22117 = CARTESIAN_POINT ( 'NONE',  ( -12.42894476027428929, -17.97759322220185396, -216.3110355466728834 ) ) ;
#22118 = CARTESIAN_POINT ( 'NONE',  ( 8.709470447750865318, -17.43408031369701661, -216.5121658579468829 ) ) ;
#22119 = CARTESIAN_POINT ( 'NONE',  ( -25.98311979368102342, 15.13734258059737670, -220.6162231662327429 ) ) ;
#22120 = CARTESIAN_POINT ( 'NONE',  ( 16.49020573214642837, 22.44566021525517741, -224.7841662740084701 ) ) ;
#22121 = CARTESIAN_POINT ( 'NONE',  ( -22.99617382825321599, 17.18101613848176967, -230.9512687019100099 ) ) ;
#22122 = CARTESIAN_POINT ( 'NONE',  ( -12.13127060986278316, 5.971392262169284315, -229.0615017441034524 ) ) ;
#22123 = CARTESIAN_POINT ( 'NONE',  ( -24.05661684749028240, -8.720095227435134433, -219.0096885115910084 ) ) ;
#22124 = ORIENTED_EDGE ( 'NONE', *, *, #16914, .T. ) ;
#22125 = CARTESIAN_POINT ( 'NONE',  ( -4.170472558179216804, 16.67407401355319152, -230.2690496885289804 ) ) ;
#22126 = CARTESIAN_POINT ( 'NONE',  ( 25.50289296650958448, 5.998088869914441901, -233.1161630295026157 ) ) ;
#22127 = CARTESIAN_POINT ( 'NONE',  ( 5.784594921161807513, 11.98867617302893329, -219.3746160931291058 ) ) ;
#22128 = CARTESIAN_POINT ( 'NONE',  ( 10.05733608402134216, -9.620616164199983444, -224.9449885650552119 ) ) ;
#22129 = DIRECTION ( 'NONE',  ( -1.000000000000000000, 0.000000000000000000, 0.000000000000000000 ) ) ;
#22130 = EDGE_LOOP ( 'NONE', ( #3012, #10702 ) ) ;
#22131 = CARTESIAN_POINT ( 'NONE',  ( -3.003186468682855104, 15.63968344752823469, -231.5301608670590667 ) ) ;
#22132 = CARTESIAN_POINT ( 'NONE',  ( -24.34656557913400476, -15.24755813437383267, -217.2726941375463809 ) ) ;
#22133 = DIRECTION ( 'NONE',  ( -1.000000000000000000, 0.000000000000000000, 0.000000000000000000 ) ) ;
#22134 = CARTESIAN_POINT ( 'NONE',  ( 22.46220731426537043, 18.23201731183003460, -227.5436199598787539 ) ) ;
#22135 = DIRECTION ( 'NONE',  ( -0.000000000000000000, -0.000000000000000000, -1.000000000000000000 ) ) ;
#22136 = CARTESIAN_POINT ( 'NONE',  ( 25.46470895113276711, -14.41152162994631070, -228.1811935238409035 ) ) ;
#22137 =( NAMED_UNIT ( * ) PLANE_ANGLE_UNIT ( ) SI_UNIT ( $, .RADIAN. ) );
#22138 = CARTESIAN_POINT ( 'NONE',  ( -23.49379658590067876, 11.46840048879614393, -217.2519070826072323 ) ) ;
#22139 = CARTESIAN_POINT ( 'NONE',  ( 17.28149325064817887, -1.074788064772476792, -229.5315781944399305 ) ) ;
#22140 = CARTESIAN_POINT ( 'NONE',  ( -13.66944713747931139, -25.56883467164384527, -222.3908458502962731 ) ) ;
#22141 = CARTESIAN_POINT ( 'NONE',  ( 18.06016678184731461, 2.257982981100609354, -218.9983079406065940 ) ) ;
#22142 = DIRECTION ( 'NONE',  ( -0.000000000000000000, -0.000000000000000000, 1.000000000000000000 ) ) ;
#22143 = CARTESIAN_POINT ( 'NONE',  ( 15.64298904066490259, -12.83894575744357880, -230.8789486217465594 ) ) ;
#22144 = CIRCLE ( 'NONE', #12089, 3.000000000000002665 ) ;
#22145 = DIRECTION ( 'NONE',  ( 0.000000000000000000, 0.000000000000000000, -1.000000000000000000 ) ) ;
#22146 = EDGE_CURVE ( 'NONE', #13000, #862, #13529, .T. ) ;
#22147 = CARTESIAN_POINT ( 'NONE',  ( 21.65362371779453454, -0.3438195010044712285, -227.9814669592245195 ) ) ;
#22148 = CARTESIAN_POINT ( 'NONE',  ( 11.73428189025226942, 12.46434742632455084, -228.1539301014595083 ) ) ;
#22149 = CARTESIAN_POINT ( 'NONE',  ( 5.079647427451626562, 16.77877517420371234, -220.7769382327915366 ) ) ;
#22150 = CARTESIAN_POINT ( 'NONE',  ( 7.820185266007354308, -13.10000580370673440, -218.6580452893993254 ) ) ;
#22151 = CARTESIAN_POINT ( 'NONE',  ( 11.14834367153813233, -21.42845646353120870, -216.4520112529555718 ) ) ;
#22152 = ORIENTED_EDGE ( 'NONE', *, *, #15077, .F. ) ;
#22153 = CARTESIAN_POINT ( 'NONE',  ( -11.48592899399814726, 13.65854631785387774, -230.8311022452805616 ) ) ;
#22154 = CARTESIAN_POINT ( 'NONE',  ( -18.90911063232017142, 5.352531560950812839, -219.6301177803536575 ) ) ;
#22155 = CARTESIAN_POINT ( 'NONE',  ( 14.65309016725241698, 3.424799466898550637, -221.5217808432381048 ) ) ;
#22156 = ORIENTED_EDGE ( 'NONE', *, *, #13389, .T. ) ;
#22157 = CARTESIAN_POINT ( 'NONE',  ( -6.911745780724915633, -15.37483479843349699, -221.7918796665217656 ) ) ;
#22158 = CARTESIAN_POINT ( 'NONE',  ( -10.35670734540881277, -3.593890535426112365, 92.00000000000001421 ) ) ;
#22159 = VERTEX_POINT ( 'NONE', #4065 ) ;
#22160 = CARTESIAN_POINT ( 'NONE',  ( 8.343316395906509086, 11.57404413652245800, -231.1403332574589911 ) ) ;
#22161 = CARTESIAN_POINT ( 'NONE',  ( 18.44909377000590922, -20.66544815256419199, -223.5047567001167863 ) ) ;
#22162 = CARTESIAN_POINT ( 'NONE',  ( 10.07175337281514871, 14.76776740066196325, -231.7834566702614723 ) ) ;
#22163 = CARTESIAN_POINT ( 'NONE',  ( -16.74550766701807447, 3.787526820511904813, -217.9802846976114381 ) ) ;
#22164 = CIRCLE ( 'NONE', #11734, 3.000000000000033751 ) ;
#22165 = CARTESIAN_POINT ( 'NONE',  ( 24.00840102751045890, 17.37402299239434100, -218.3110108534040137 ) ) ;
#22166 = CARTESIAN_POINT ( 'NONE',  ( -24.19163806436329978, 8.131440952769249719, -230.9341214615949127 ) ) ;
#22167 = CARTESIAN_POINT ( 'NONE',  ( -0.1571923090946999446, 19.34188126963334398, -216.6893131123363787 ) ) ;
#22168 = DIRECTION ( 'NONE',  ( 1.000000000000000000, 6.982962677686272233E-15, 0.000000000000000000 ) ) ;
#22169 = CARTESIAN_POINT ( 'NONE',  ( 5.668262076144046979, -25.28042871382391965, -216.8182873783340483 ) ) ;
#22170 = CARTESIAN_POINT ( 'NONE',  ( 20.89700225552940793, -4.547446057044195911, -232.3806459760843666 ) ) ;
#22171 = CARTESIAN_POINT ( 'NONE',  ( 0.000000000000000000, -25.00000000000000000, -75.00000000000000000 ) ) ;
#22172 = FACE_OUTER_BOUND ( 'NONE', #6857, .T. ) ;
#22173 = CARTESIAN_POINT ( 'NONE',  ( 24.58316096239279602, 5.861425670879941485, -231.3104446318280623 ) ) ;
#22174 = CARTESIAN_POINT ( 'NONE',  ( -24.24026017931571175, -14.11860166261188354, -224.3835235244768569 ) ) ;
#22175 = DIRECTION ( 'NONE',  ( -0.000000000000000000, -0.000000000000000000, 1.000000000000000000 ) ) ;
#22176 = CARTESIAN_POINT ( 'NONE',  ( 5.377793152941013233, -17.45375835550001753, -231.2474386379397231 ) ) ;
#22177 = CARTESIAN_POINT ( 'NONE',  ( 29.81944548462877975, 8.043843257819576209, -228.1755181449411793 ) ) ;
#22178 = CARTESIAN_POINT ( 'NONE',  ( -10.30870167223346456, 11.95603877111467561, -228.4123369090513336 ) ) ;
#22179 = CARTESIAN_POINT ( 'NONE',  ( -9.964021556040458805, 12.25789996591640119, -217.8262340283327774 ) ) ;
#22180 = EDGE_LOOP ( 'NONE', ( #6327, #5035, #2086, #13609 ) ) ;
#22181 = CARTESIAN_POINT ( 'NONE',  ( 16.57791564354289093, -3.035441731457511949, -233.7002882787241163 ) ) ;
#22182 = ORIENTED_EDGE ( 'NONE', *, *, #13528, .T. ) ;
#22183 = CARTESIAN_POINT ( 'NONE',  ( 11.67669251569587985, 24.04736029062789981, -218.5856804285192254 ) ) ;
#22184 = EDGE_CURVE ( 'NONE', #3468, #15083, #14763, .T. ) ;
#22185 = CARTESIAN_POINT ( 'NONE',  ( -15.51814470728089645, 2.949994979016113739, -222.8331727603033130 ) ) ;
#22186 = CARTESIAN_POINT ( 'NONE',  ( 18.50073117969547098, -1.889592114545683987, -232.6396648696776026 ) ) ;
#22187 = LINE ( 'NONE', #13756, #18100 ) ;
#22188 = CARTESIAN_POINT ( 'NONE',  ( 8.903385417657583289, 10.41040586594612272, -227.6527940987422198 ) ) ;
#22189 = CARTESIAN_POINT ( 'NONE',  ( -22.19349712985372491, 11.03542788991621748, -219.7744882786627443 ) ) ;
#22190 = CARTESIAN_POINT ( 'NONE',  ( 1.773237071419721422, 13.09828209437875302, -220.6531024550077404 ) ) ;
#22191 = EDGE_CURVE ( 'NONE', #12695, #21649, #10280, .T. ) ;
#22192 = CARTESIAN_POINT ( 'NONE',  ( 13.59483335902903178, 5.678732573479117640, -228.5032236586631313 ) ) ;
#22193 = CARTESIAN_POINT ( 'NONE',  ( -9.208465596459861402, -9.574166310164313742, -220.4340298767933177 ) ) ;
#22194 = ORIENTED_EDGE ( 'NONE', *, *, #5979, .T. ) ;
#22195 = CARTESIAN_POINT ( 'NONE',  ( -11.96638064467250473, -24.81952708901905069, -229.8544473269683692 ) ) ;
#22196 = CARTESIAN_POINT ( 'NONE',  ( -8.653738780971721667, 11.12943719949617893, -219.7525355316396087 ) ) ;
#22197 = CARTESIAN_POINT ( 'NONE',  ( 7.021536848793814123, -14.49751826649810482, -218.4909385705359455 ) ) ;
#22198 = CARTESIAN_POINT ( 'NONE',  ( -2.698926868850080041, 12.89339462271858316, -226.7595176699009585 ) ) ;
#22199 = CARTESIAN_POINT ( 'NONE',  ( 19.25263663724807728, -8.631913731826720948, -234.6583132812941983 ) ) ;
#22200 = CARTESIAN_POINT ( 'NONE',  ( -13.21314811618155716, -9.038438575223175064, -230.6430079410957603 ) ) ;
#22201 = CARTESIAN_POINT ( 'NONE',  ( 8.778334628954494789, 12.71782457734010841, -222.1923057070808909 ) ) ;
#22202 = CARTESIAN_POINT ( 'NONE',  ( 0.000000000000000000, 0.000000000000000000, -105.0000000000000000 ) ) ;
#22203 = CARTESIAN_POINT ( 'NONE',  ( -9.115411286166651195, 13.66191091052436235, -230.3338332872444312 ) ) ;
#22204 = CARTESIAN_POINT ( 'NONE',  ( 13.64836464229338198, 15.83060743948028737, -232.0893758582176929 ) ) ;
#22205 = CARTESIAN_POINT ( 'NONE',  ( 14.32085100525799248, 9.220655089380342062, -219.9006227404039464 ) ) ;
#22206 = CARTESIAN_POINT ( 'NONE',  ( 20.54489901492447501, 10.52141067440427591, -216.2005526543161693 ) ) ;
#22207 = CARTESIAN_POINT ( 'NONE',  ( 6.835279263914467052, -26.27742004305391177, -233.7345821414606348 ) ) ;
#22208 = CARTESIAN_POINT ( 'NONE',  ( -3.712761995161701911, 23.50704853188985766, -216.1220552374512067 ) ) ;
#22209 = DIRECTION ( 'NONE',  ( -1.000000000000000000, 0.000000000000000000, 0.000000000000000000 ) ) ;
#22210 = CARTESIAN_POINT ( 'NONE',  ( 13.96153919378708075, -19.04487818418218481, -231.5728976975466367 ) ) ;
#22211 = CARTESIAN_POINT ( 'NONE',  ( -15.36327147092456791, 5.453733681707060299, -220.0043800961136355 ) ) ;
#22212 = CARTESIAN_POINT ( 'NONE',  ( -1.772400894765090662, 19.49811434610897010, -217.8797837662441168 ) ) ;
#22213 = CARTESIAN_POINT ( 'NONE',  ( -11.39823187951283501, -7.998194509987097689, -226.8062974464413912 ) ) ;
#22214 = CARTESIAN_POINT ( 'NONE',  ( -24.92290506463145405, 6.124412323591598373, -220.3779252408000104 ) ) ;
#22215 = EDGE_CURVE ( 'NONE', #17518, #7303, #19803, .T. ) ;
#22216 = CARTESIAN_POINT ( 'NONE',  ( 12.03015173539790617, 23.46358517874481109, -216.0611092640310744 ) ) ;
#22217 = VERTEX_POINT ( 'NONE', #802 ) ;
#22218 = CARTESIAN_POINT ( 'NONE',  ( 13.43170911749896490, 19.07691563292472026, -232.7497845103644636 ) ) ;
#22219 = CARTESIAN_POINT ( 'NONE',  ( 13.38912848839664704, -8.011079660592983487, -223.8512906815321628 ) ) ;
#22220 = CARTESIAN_POINT ( 'NONE',  ( 15.91397826126795323, -3.183288324723350549, -218.2846031002558504 ) ) ;
#22221 = DIRECTION ( 'NONE',  ( -1.000000000000000000, 0.000000000000000000, 0.000000000000000000 ) ) ;
#22222 = CARTESIAN_POINT ( 'NONE',  ( -1.249406995060579062, 25.48934319316224162, -216.9406480707515072 ) ) ;
#22223 = CARTESIAN_POINT ( 'NONE',  ( -17.20514689733751368, -7.568958929800959190, -215.6459182133127115 ) ) ;
#22224 = CARTESIAN_POINT ( 'NONE',  ( -3.734153817218577309, -19.72686645808614614, -233.9207428641194610 ) ) ;
#22225 = CARTESIAN_POINT ( 'NONE',  ( 6.260999666360449467, -13.19315344885661645, -220.2890618333529744 ) ) ;
#22226 = CARTESIAN_POINT ( 'NONE',  ( -10.94147694953847250, 13.90730769817462864, -218.7797619932150042 ) ) ;
#22227 = CARTESIAN_POINT ( 'NONE',  ( 14.72046356508972309, 21.23077830076469041, -229.4562045376679578 ) ) ;
#22228 = CARTESIAN_POINT ( 'NONE',  ( -25.61997837663875188, 10.01664178086244483, -231.6711741719404074 ) ) ;
#22229 = CARTESIAN_POINT ( 'NONE',  ( -11.30246491834384770, 5.534029070539333794, -225.8243940897388597 ) ) ;
#22230 = CARTESIAN_POINT ( 'NONE',  ( -23.21124258271143503, -15.80671483884278317, -224.0808897361354468 ) ) ;
#22231 = ORIENTED_EDGE ( 'NONE', *, *, #18082, .T. ) ;
#22232 = CARTESIAN_POINT ( 'NONE',  ( -11.16203726658389606, 26.27101666727781648, -227.8592829514190612 ) ) ;
#22233 = CARTESIAN_POINT ( 'NONE',  ( 20.10109416526603709, 2.018147939476731434, -216.1034161917718848 ) ) ;
#22234 = CARTESIAN_POINT ( 'NONE',  ( 17.60070748514786132, 25.68479983175475567, -229.9331108608050158 ) ) ;
#22235 = AXIS2_PLACEMENT_3D ( 'NONE', #17071, #13468, #20307 ) ;
#22236 = CARTESIAN_POINT ( 'NONE',  ( 11.29822263435752205, -11.23247557268489771, -230.2410575525588570 ) ) ;
#22237 = FACE_OUTER_BOUND ( 'NONE', #3153, .T. ) ;
#22238 = EDGE_LOOP ( 'NONE', ( #5042, #12479, #1180, #5387 ) ) ;
#22239 = CARTESIAN_POINT ( 'NONE',  ( 0.4042326456706432647, 15.50845657815858303, -219.2680337625893401 ) ) ;
#22240 = CARTESIAN_POINT ( 'NONE',  ( -21.94322237485859972, -13.31528874885349900, -215.4027562252440759 ) ) ;
#22241 = DIRECTION ( 'NONE',  ( 1.000000000000000000, 0.000000000000000000, 0.000000000000000000 ) ) ;
#22242 = CARTESIAN_POINT ( 'NONE',  ( 16.84848658399567611, 11.39632653812981644, -217.9589513831453473 ) ) ;
#22243 = CARTESIAN_POINT ( 'NONE',  ( -28.59157645096996347, 5.137867505054540374, -220.4667042235044505 ) ) ;
#22244 = CARTESIAN_POINT ( 'NONE',  ( 9.584731462935641488, -12.36622837314704348, -230.4796538097028531 ) ) ;
#22245 = CARTESIAN_POINT ( 'NONE',  ( -28.99926036811508467, 3.909990568804979194, -228.9613767892386988 ) ) ;
#22246 = CARTESIAN_POINT ( 'NONE',  ( 12.91815243135930480, 5.607966342865584153, -224.2227256053222959 ) ) ;
#22247 = CARTESIAN_POINT ( 'NONE',  ( -1.981531036097845533, -15.05108582582333909, -227.0172948689592829 ) ) ;
#22248 = CARTESIAN_POINT ( 'NONE',  ( 14.19800769603076240, 4.587407146151301518, -224.2928935459285071 ) ) ;
#22249 = DIRECTION ( 'NONE',  ( -1.000000000000000000, 0.000000000000000000, 0.000000000000000000 ) ) ;
#22250 = CARTESIAN_POINT ( 'NONE',  ( 14.67088464789753388, -9.947482835004686663, -220.6944058341955497 ) ) ;
#22251 = CARTESIAN_POINT ( 'NONE',  ( 14.76992028084322683, -2.175943223131179494, -227.0668203386748019 ) ) ;
#22252 = CARTESIAN_POINT ( 'NONE',  ( -20.87413353426600438, -9.658245891971773744, 2.612681058926761946 ) ) ;
#22253 = CARTESIAN_POINT ( 'NONE',  ( 12.60818910183731489, 13.02403301690871729, -229.3305689548085695 ) ) ;
#22254 = CARTESIAN_POINT ( 'NONE',  ( 3.522445101072706475, 23.08420003150784439, -231.7850044194335055 ) ) ;
#22255 = CARTESIAN_POINT ( 'NONE',  ( 15.68748001070188458, -20.89997441943167900, -216.2583427777263125 ) ) ;
#22256 = CARTESIAN_POINT ( 'NONE',  ( 6.053458391837899910, -12.85229775019162268, -220.9645494416007523 ) ) ;
#22257 = CARTESIAN_POINT ( 'NONE',  ( -14.94618804342693075, 22.09718979644185666, -219.6454806548149463 ) ) ;
#22258 = CARTESIAN_POINT ( 'NONE',  ( -16.03353370602922467, 4.897644413504528060, -222.5335369890782999 ) ) ;
#22259 = CARTESIAN_POINT ( 'NONE',  ( 14.72648027392381387, 10.15511732729369676, -229.5776536674053716 ) ) ;
#22260 = CARTESIAN_POINT ( 'NONE',  ( -6.877419757825867563, -14.31154863906730412, -224.3431884172090918 ) ) ;
#22261 = CARTESIAN_POINT ( 'NONE',  ( -6.938893903907228378E-15, 0.000000000000000000, -224.9999999999999716 ) ) ;
#22262 = VERTEX_POINT ( 'NONE', #11491 ) ;
#22263 = CARTESIAN_POINT ( 'NONE',  ( 15.28706223449149348, 2.473424253736659306, -227.9634568993954531 ) ) ;
#22264 = CARTESIAN_POINT ( 'NONE',  ( 11.60500945006145024, -11.05507752957471190, -226.0500390094313730 ) ) ;
#22265 = CARTESIAN_POINT ( 'NONE',  ( -6.938893903907228378E-15, 0.000000000000000000, -224.9999999999999716 ) ) ;
#22266 = NEXT_ASSEMBLY_USAGE_OCCURRENCE ( 'NAUO1', ' ', ' ', #110, #8374, $ ) ;
#22267 = NEXT_ASSEMBLY_USAGE_OCCURRENCE ( 'NAUO2', ' ', ' ', #110, #5050, $ ) ;
#22268 = NEXT_ASSEMBLY_USAGE_OCCURRENCE ( 'NAUO3', ' ', ' ', #110, #16346, $ ) ;
#22269 = NEXT_ASSEMBLY_USAGE_OCCURRENCE ( 'NAUO4', ' ', ' ', #110, #6018, $ ) ;
#22270 = NEXT_ASSEMBLY_USAGE_OCCURRENCE ( 'NAUO5', ' ', ' ', #110, #6428, $ ) ;
#22271 = NEXT_ASSEMBLY_USAGE_OCCURRENCE ( 'NAUO6', ' ', ' ', #110, #14016, $ ) ;
#22272 = NEXT_ASSEMBLY_USAGE_OCCURRENCE ( 'NAUO7', ' ', ' ', #110, #17443, $ ) ;
#22273 = NEXT_ASSEMBLY_USAGE_OCCURRENCE ( 'NAUO8', ' ', ' ', #110, #7130, $ ) ;
ENDSEC;
END-ISO-10303-21;
